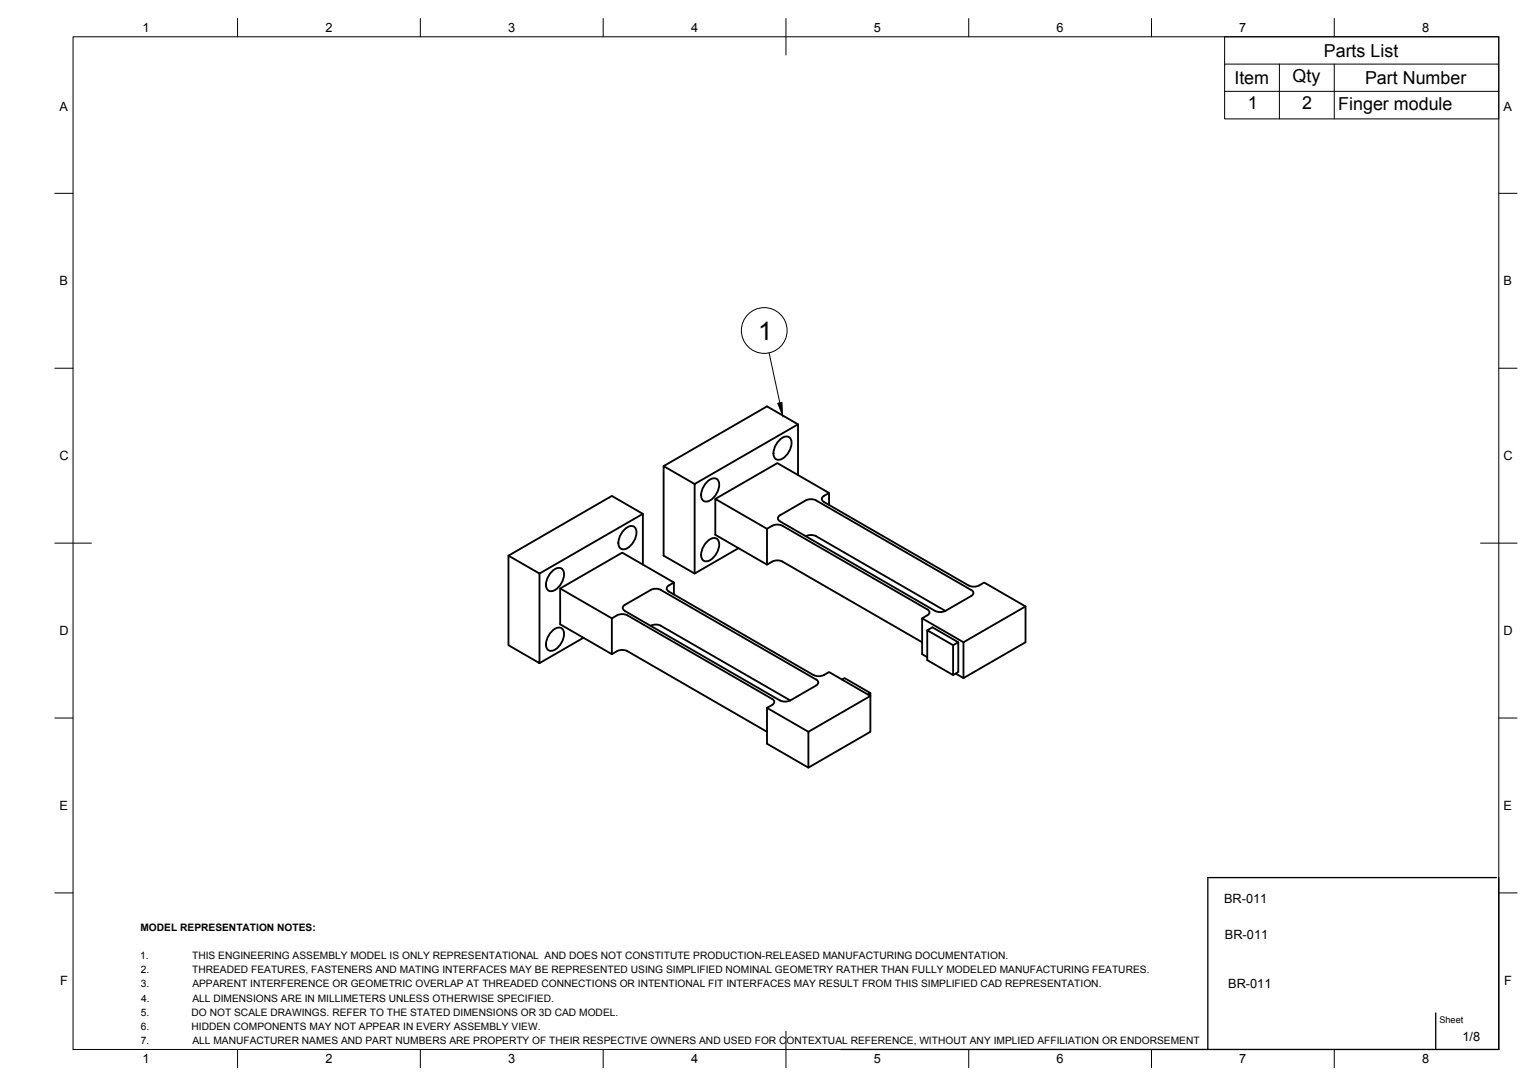
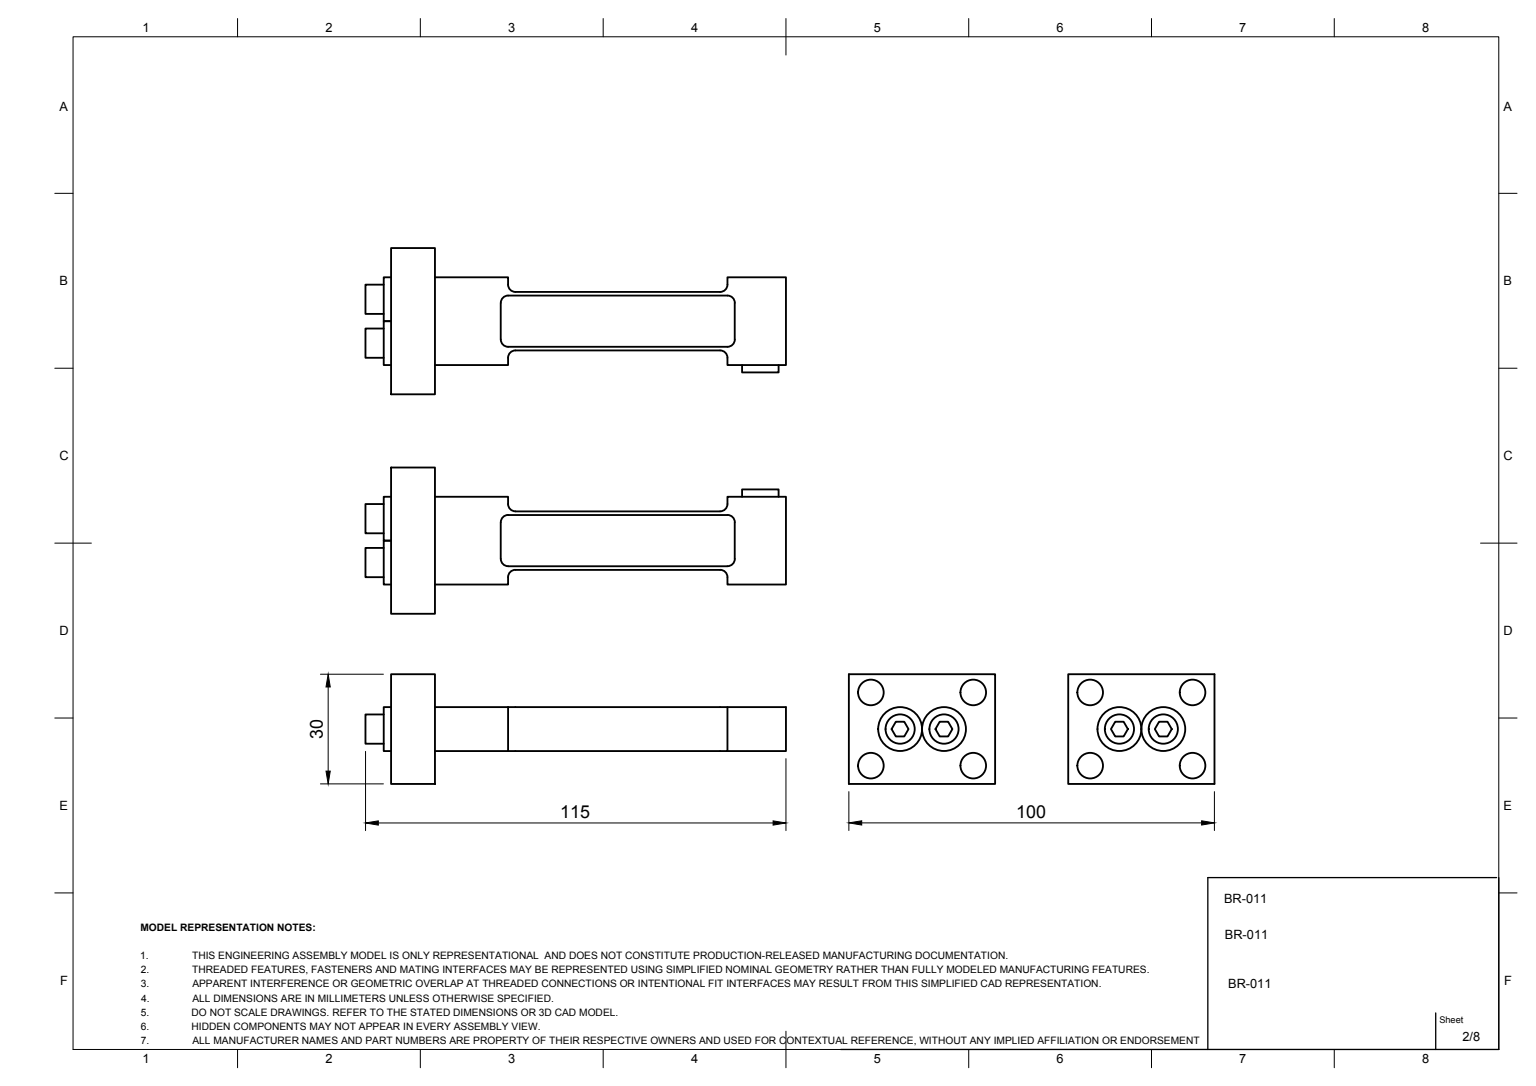
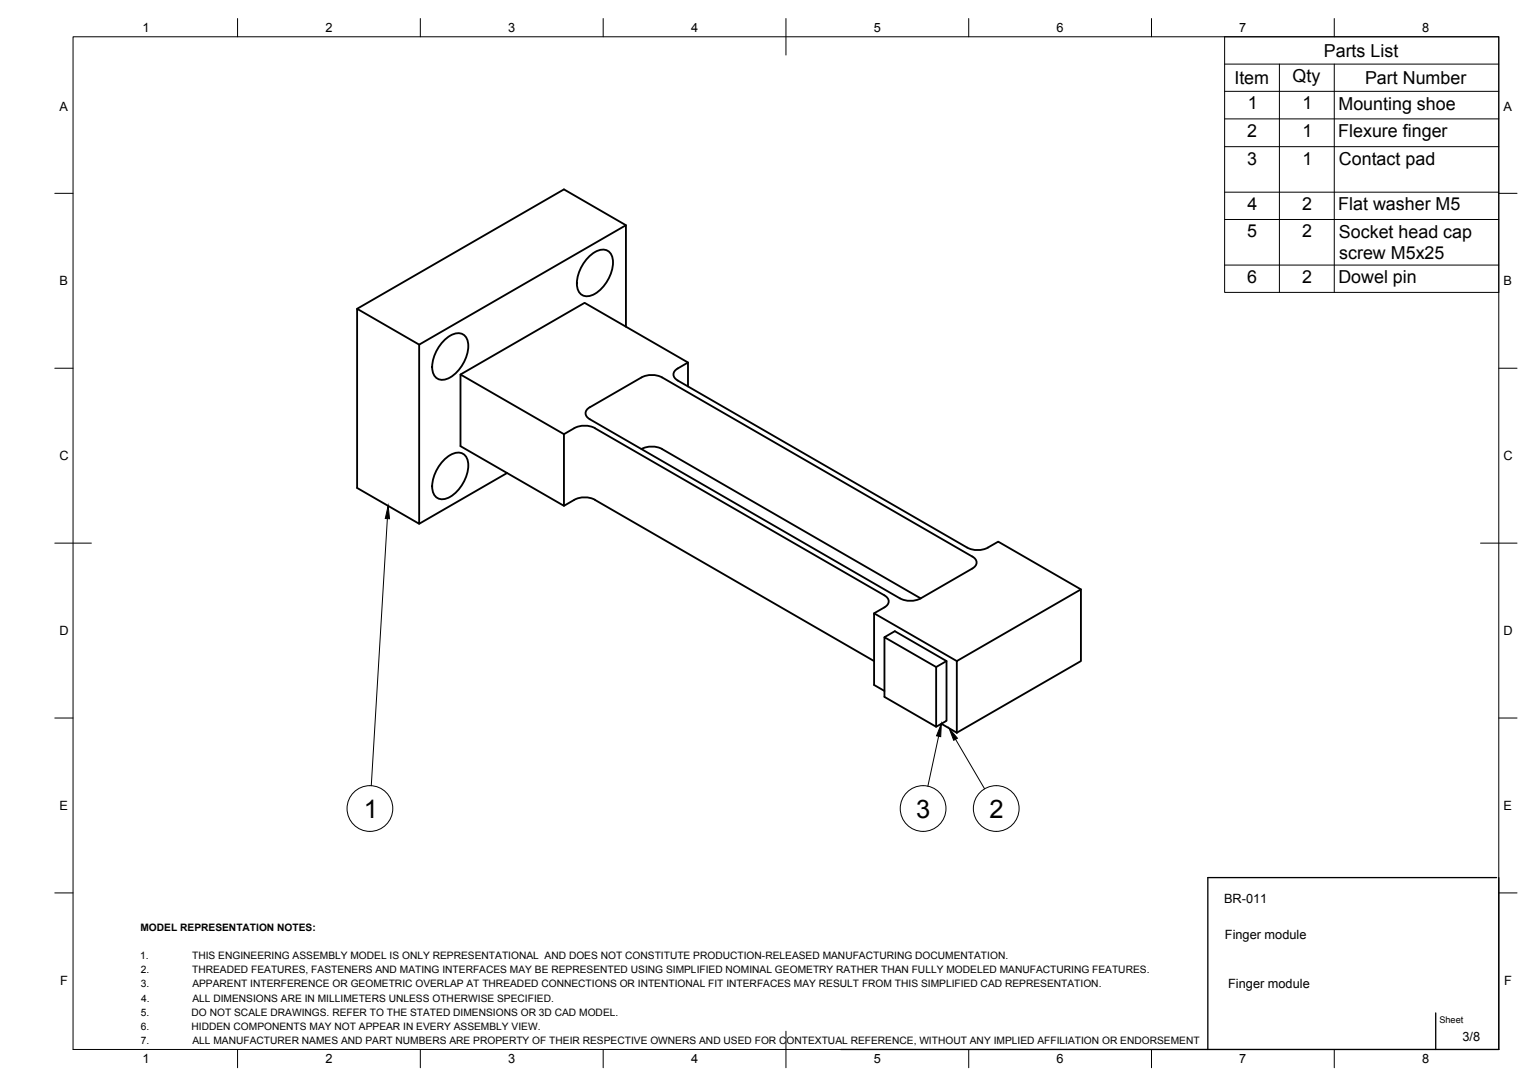
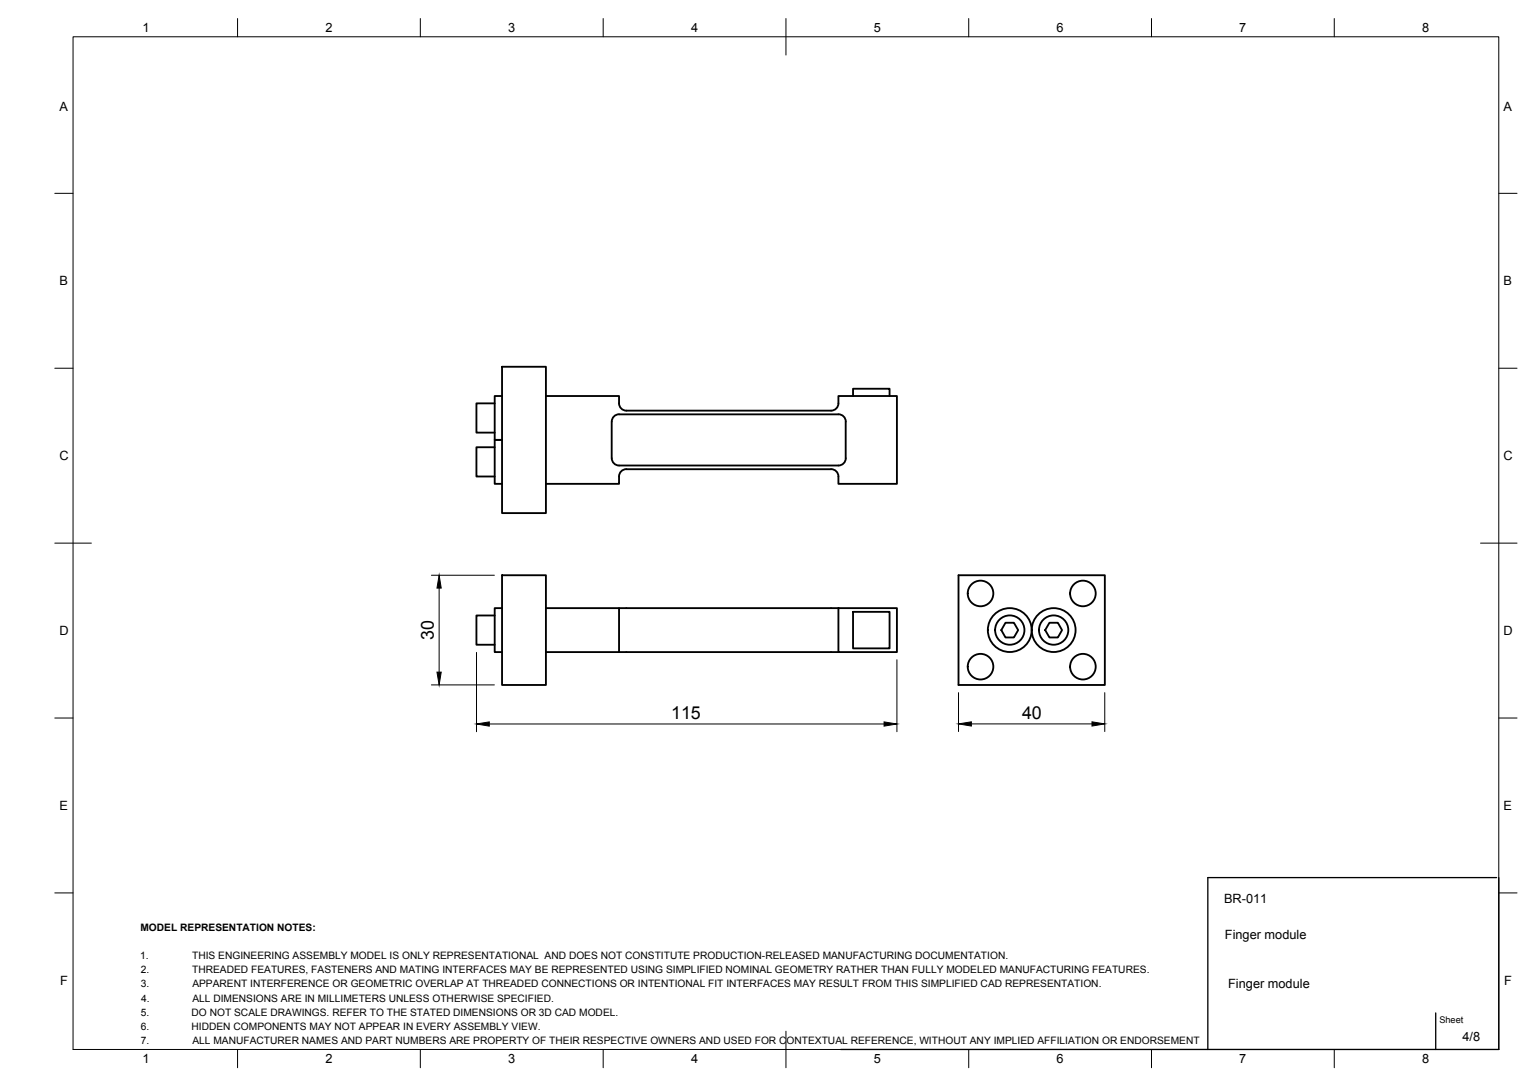
ISO-10303-21;
HEADER;
/* Generated by software containing ST-Developer
 * from STEP Tools, Inc. (www.steptools.com) 
 */

FILE_DESCRIPTION(
/* description */ ('Independent pair of monolithic parallel-leaf compliant finger modules.
 Shared native part/module instances; external gripper actuator outsid
e scope. Whole-mm geometry,1mm webs,56mm straight span,12mm depth,32mm
 nominal contact gap. Undeformed CAD reference; material condition, el
astic range, fatigue and gripping force unassigned.'),
/* implementation_level */ '2;1');

FILE_NAME(
/* name */ 'BR-011.step',
/* time_stamp */ '2026-11-07T22:36:16-08:00',
/* author */ (''),
/* organization */ (''),
/* preprocessor_version */ 'ST-DEVELOPER v20.2',
/* originating_system */ 'Autodesk Translation Framework v15.17.0.0',
/* authorisation */ '');

FILE_SCHEMA (('AUTOMOTIVE_DESIGN { 1 0 10303 214 3 1 1 }'));
ENDSEC;

DATA;
#10=MECHANICAL_DESIGN_GEOMETRIC_PRESENTATION_REPRESENTATION('',(#329,#330,
#331,#332,#333,#334),#13801);
#11=ITEM_DEFINED_TRANSFORMATION($,$,#3769,#4029);
#12=ITEM_DEFINED_TRANSFORMATION($,$,#3802,#4030);
#13=ITEM_DEFINED_TRANSFORMATION($,$,#3925,#4031);
#14=ITEM_DEFINED_TRANSFORMATION($,$,#3932,#4032);
#15=ITEM_DEFINED_TRANSFORMATION($,$,#3941,#4033);
#16=ITEM_DEFINED_TRANSFORMATION($,$,#4023,#4034);
#17=ITEM_DEFINED_TRANSFORMATION($,$,#3932,#4035);
#18=ITEM_DEFINED_TRANSFORMATION($,$,#3941,#4036);
#19=ITEM_DEFINED_TRANSFORMATION($,$,#4023,#4037);
#20=ITEM_DEFINED_TRANSFORMATION($,$,#3768,#4038);
#21=ITEM_DEFINED_TRANSFORMATION($,$,#3768,#4039);
#22=(
REPRESENTATION_RELATIONSHIP($,$,#13835,#13834)
REPRESENTATION_RELATIONSHIP_WITH_TRANSFORMATION(#11)
SHAPE_REPRESENTATION_RELATIONSHIP()
);
#23=(
REPRESENTATION_RELATIONSHIP($,$,#13836,#13834)
REPRESENTATION_RELATIONSHIP_WITH_TRANSFORMATION(#12)
SHAPE_REPRESENTATION_RELATIONSHIP()
);
#24=(
REPRESENTATION_RELATIONSHIP($,$,#13837,#13834)
REPRESENTATION_RELATIONSHIP_WITH_TRANSFORMATION(#13)
SHAPE_REPRESENTATION_RELATIONSHIP()
);
#25=(
REPRESENTATION_RELATIONSHIP($,$,#13838,#13834)
REPRESENTATION_RELATIONSHIP_WITH_TRANSFORMATION(#14)
SHAPE_REPRESENTATION_RELATIONSHIP()
);
#26=(
REPRESENTATION_RELATIONSHIP($,$,#13839,#13834)
REPRESENTATION_RELATIONSHIP_WITH_TRANSFORMATION(#15)
SHAPE_REPRESENTATION_RELATIONSHIP()
);
#27=(
REPRESENTATION_RELATIONSHIP($,$,#13840,#13834)
REPRESENTATION_RELATIONSHIP_WITH_TRANSFORMATION(#16)
SHAPE_REPRESENTATION_RELATIONSHIP()
);
#28=(
REPRESENTATION_RELATIONSHIP($,$,#13838,#13834)
REPRESENTATION_RELATIONSHIP_WITH_TRANSFORMATION(#17)
SHAPE_REPRESENTATION_RELATIONSHIP()
);
#29=(
REPRESENTATION_RELATIONSHIP($,$,#13839,#13834)
REPRESENTATION_RELATIONSHIP_WITH_TRANSFORMATION(#18)
SHAPE_REPRESENTATION_RELATIONSHIP()
);
#30=(
REPRESENTATION_RELATIONSHIP($,$,#13840,#13834)
REPRESENTATION_RELATIONSHIP_WITH_TRANSFORMATION(#19)
SHAPE_REPRESENTATION_RELATIONSHIP()
);
#31=(
REPRESENTATION_RELATIONSHIP($,$,#13834,#13833)
REPRESENTATION_RELATIONSHIP_WITH_TRANSFORMATION(#20)
SHAPE_REPRESENTATION_RELATIONSHIP()
);
#32=(
REPRESENTATION_RELATIONSHIP($,$,#13834,#13833)
REPRESENTATION_RELATIONSHIP_WITH_TRANSFORMATION(#21)
SHAPE_REPRESENTATION_RELATIONSHIP()
);
#33=CONTEXT_DEPENDENT_SHAPE_REPRESENTATION(#22,#13822);
#34=CONTEXT_DEPENDENT_SHAPE_REPRESENTATION(#23,#13823);
#35=CONTEXT_DEPENDENT_SHAPE_REPRESENTATION(#24,#13824);
#36=CONTEXT_DEPENDENT_SHAPE_REPRESENTATION(#25,#13825);
#37=CONTEXT_DEPENDENT_SHAPE_REPRESENTATION(#26,#13826);
#38=CONTEXT_DEPENDENT_SHAPE_REPRESENTATION(#27,#13827);
#39=CONTEXT_DEPENDENT_SHAPE_REPRESENTATION(#28,#13828);
#40=CONTEXT_DEPENDENT_SHAPE_REPRESENTATION(#29,#13829);
#41=CONTEXT_DEPENDENT_SHAPE_REPRESENTATION(#30,#13830);
#42=CONTEXT_DEPENDENT_SHAPE_REPRESENTATION(#31,#13831);
#43=CONTEXT_DEPENDENT_SHAPE_REPRESENTATION(#32,#13832);
#44=NEXT_ASSEMBLY_USAGE_OCCURRENCE('Mounting shoe:1','Mounting shoe:1',
'Mounting shoe:1',#13843,#13844,'Mounting shoe:1');
#45=NEXT_ASSEMBLY_USAGE_OCCURRENCE('Flexure finger:1',
'Flexure finger:1','Flexure finger:1',#13843,#13845,'Flexure finger:1');
#46=NEXT_ASSEMBLY_USAGE_OCCURRENCE('Contact pad:1','Contact pad:1',
'Contact pad:1',#13843,#13846,'Contact pad:1');
#47=NEXT_ASSEMBLY_USAGE_OCCURRENCE('Flat washer M5:1',
'Flat washer M5:1','Flat washer M5:1',#13843,#13847,'Flat washer M5:1');
#48=NEXT_ASSEMBLY_USAGE_OCCURRENCE('Socket head cap screw M5x25:1',
'Socket head cap screw M5x25:1','Socket head cap screw M5x25:1',#13843,
#13848,'Socket head cap screw M5x25:1');
#49=NEXT_ASSEMBLY_USAGE_OCCURRENCE('Dowel pin:1','Dowel pin:1',
'Dowel pin:1',#13843,#13849,'Dowel pin:1');
#50=NEXT_ASSEMBLY_USAGE_OCCURRENCE('Flat washer M5:2',
'Flat washer M5:2','Flat washer M5:2',#13843,#13847,'Flat washer M5:2');
#51=NEXT_ASSEMBLY_USAGE_OCCURRENCE('Socket head cap screw M5x25:2',
'Socket head cap screw M5x25:2','Socket head cap screw M5x25:2',#13843,
#13848,'Socket head cap screw M5x25:2');
#52=NEXT_ASSEMBLY_USAGE_OCCURRENCE('Dowel pin:2','Dowel pin:2',
'Dowel pin:2',#13843,#13849,'Dowel pin:2');
#53=NEXT_ASSEMBLY_USAGE_OCCURRENCE('Finger module:1','Finger module:1',
'Finger module:1',#13842,#13843,'Finger module:1');
#54=NEXT_ASSEMBLY_USAGE_OCCURRENCE('Finger module:2','Finger module:2',
'Finger module:2',#13842,#13843,'Finger module:2');
#55=CONICAL_SURFACE('',#4004,2.,0.785398163397448);
#56=B_SPLINE_SURFACE_WITH_KNOTS('',3,3,((#7071,#7072,#7073,#7074,#7075,
#7076,#7077,#7078,#7079,#7080,#7081,#7082,#7083,#7084,#7085,#7086,#7087,
#7088,#7089,#7090,#7091,#7092,#7093,#7094,#7095,#7096,#7097,#7098,#7099,
#7100,#7101,#7102,#7103,#7104,#7105,#7106,#7107,#7108,#7109,#7110,#7111,
#7112,#7113,#7114,#7115,#7116,#7117,#7118,#7119,#7120,#7121,#7122,#7123,
#7124,#7125,#7126,#7127,#7128,#7129,#7130,#7131,#7132,#7133,#7134,#7135,
#7136,#7137,#7138,#7139,#7140,#7141,#7142,#7143,#7144,#7145,#7146,#7147,
#7148,#7149,#7150,#7151,#7152,#7153,#7154,#7155,#7156,#7157,#7158,#7159,
#7160,#7161,#7162),(#7163,#7164,#7165,#7166,#7167,#7168,#7169,#7170,#7171,
#7172,#7173,#7174,#7175,#7176,#7177,#7178,#7179,#7180,#7181,#7182,#7183,
#7184,#7185,#7186,#7187,#7188,#7189,#7190,#7191,#7192,#7193,#7194,#7195,
#7196,#7197,#7198,#7199,#7200,#7201,#7202,#7203,#7204,#7205,#7206,#7207,
#7208,#7209,#7210,#7211,#7212,#7213,#7214,#7215,#7216,#7217,#7218,#7219,
#7220,#7221,#7222,#7223,#7224,#7225,#7226,#7227,#7228,#7229,#7230,#7231,
#7232,#7233,#7234,#7235,#7236,#7237,#7238,#7239,#7240,#7241,#7242,#7243,
#7244,#7245,#7246,#7247,#7248,#7249,#7250,#7251,#7252,#7253,#7254),(#7255,
#7256,#7257,#7258,#7259,#7260,#7261,#7262,#7263,#7264,#7265,#7266,#7267,
#7268,#7269,#7270,#7271,#7272,#7273,#7274,#7275,#7276,#7277,#7278,#7279,
#7280,#7281,#7282,#7283,#7284,#7285,#7286,#7287,#7288,#7289,#7290,#7291,
#7292,#7293,#7294,#7295,#7296,#7297,#7298,#7299,#7300,#7301,#7302,#7303,
#7304,#7305,#7306,#7307,#7308,#7309,#7310,#7311,#7312,#7313,#7314,#7315,
#7316,#7317,#7318,#7319,#7320,#7321,#7322,#7323,#7324,#7325,#7326,#7327,
#7328,#7329,#7330,#7331,#7332,#7333,#7334,#7335,#7336,#7337,#7338,#7339,
#7340,#7341,#7342,#7343,#7344,#7345,#7346),(#7347,#7348,#7349,#7350,#7351,
#7352,#7353,#7354,#7355,#7356,#7357,#7358,#7359,#7360,#7361,#7362,#7363,
#7364,#7365,#7366,#7367,#7368,#7369,#7370,#7371,#7372,#7373,#7374,#7375,
#7376,#7377,#7378,#7379,#7380,#7381,#7382,#7383,#7384,#7385,#7386,#7387,
#7388,#7389,#7390,#7391,#7392,#7393,#7394,#7395,#7396,#7397,#7398,#7399,
#7400,#7401,#7402,#7403,#7404,#7405,#7406,#7407,#7408,#7409,#7410,#7411,
#7412,#7413,#7414,#7415,#7416,#7417,#7418,#7419,#7420,#7421,#7422,#7423,
#7424,#7425,#7426,#7427,#7428,#7429,#7430,#7431,#7432,#7433,#7434,#7435,
#7436,#7437,#7438)),.UNSPECIFIED.,.F.,.F.,.F.,(4,4),(4,1,1,1,1,1,1,1,1,
1,1,1,1,1,1,1,1,1,1,1,1,1,1,1,1,1,1,1,1,1,1,1,1,1,1,1,1,1,1,1,1,1,1,1,1,
1,1,1,1,1,1,1,1,1,1,1,1,1,1,1,1,1,1,1,1,1,1,1,1,1,1,1,1,1,1,1,1,1,1,1,1,
1,1,1,1,1,1,1,1,4),(0.,0.0511532338502008),(11.8669242345263,12.8602116589039,
13.8534990832815,14.8467865076592,15.8400739320368,16.8333613564144,17.826648780792,
18.8199362051697,19.8132236295473,20.8065110539249,21.7997984783025,22.7930859026802,
23.7863733270578,24.7796607514354,25.772948175813,26.7662356001907,27.7595230245683,
28.7528104489459,29.7460978733235,30.7393852977012,31.7326727220788,32.7259601464564,
33.719247570834,34.7125349952117,35.7058224195893,36.6991098439669,37.6923972683445,
38.6856846927222,39.6789721170998,40.6722595414774,41.6655469658551,42.6588343902327,
43.6521218146103,44.6454092389879,45.6386966633656,46.6319840877432,47.6252715121208,
48.6185589364984,49.6118463608761,50.6051337852537,51.5984212096313,52.5917086340089,
53.5849960583866,54.5782834827642,55.5715709071418,56.5648583315194,57.5581457558971,
58.5514331802747,59.5447206046523,60.5380080290299,61.5312954534076,62.5245828777852,
63.5178703021628,64.5111577265404,65.5044451509181,66.4977325752957,67.4910199996733,
68.4843074240509,69.4775948484286,70.4708822728062,71.4641696971838,72.4574571215614,
73.4507445459391,74.4440319703167,75.4373193946943,76.430606819072,77.4238942434496,
78.4171816678272,79.4104690922048,80.4037565165825,81.3970439409601,82.3903313653377,
83.3836187897153,84.376906214093,85.3701936384706,86.3634810628482,87.3567684872258,
88.3500559116035,89.3433433359811,90.3366307603587,91.3299181847363,92.323205609114,
93.3164930334916,94.3097804578692,95.3030678822468,96.2963553066245,97.2896427310021,
98.2829301553797,99.2762175797573,100.269505004135),.UNSPECIFIED.);
#57=B_SPLINE_SURFACE_WITH_KNOTS('',3,3,((#7555,#7556,#7557,#7558,#7559,
#7560,#7561,#7562,#7563,#7564,#7565,#7566,#7567,#7568,#7569,#7570,#7571,
#7572,#7573,#7574,#7575,#7576,#7577,#7578,#7579,#7580,#7581,#7582,#7583,
#7584,#7585,#7586,#7587,#7588,#7589,#7590,#7591,#7592,#7593,#7594,#7595,
#7596,#7597,#7598,#7599,#7600,#7601,#7602,#7603,#7604,#7605,#7606,#7607,
#7608,#7609,#7610,#7611,#7612,#7613,#7614,#7615,#7616,#7617,#7618,#7619,
#7620,#7621,#7622,#7623,#7624,#7625,#7626,#7627,#7628,#7629,#7630,#7631,
#7632,#7633,#7634,#7635,#7636,#7637,#7638,#7639,#7640,#7641,#7642,#7643,
#7644,#7645,#7646),(#7647,#7648,#7649,#7650,#7651,#7652,#7653,#7654,#7655,
#7656,#7657,#7658,#7659,#7660,#7661,#7662,#7663,#7664,#7665,#7666,#7667,
#7668,#7669,#7670,#7671,#7672,#7673,#7674,#7675,#7676,#7677,#7678,#7679,
#7680,#7681,#7682,#7683,#7684,#7685,#7686,#7687,#7688,#7689,#7690,#7691,
#7692,#7693,#7694,#7695,#7696,#7697,#7698,#7699,#7700,#7701,#7702,#7703,
#7704,#7705,#7706,#7707,#7708,#7709,#7710,#7711,#7712,#7713,#7714,#7715,
#7716,#7717,#7718,#7719,#7720,#7721,#7722,#7723,#7724,#7725,#7726,#7727,
#7728,#7729,#7730,#7731,#7732,#7733,#7734,#7735,#7736,#7737,#7738),(#7739,
#7740,#7741,#7742,#7743,#7744,#7745,#7746,#7747,#7748,#7749,#7750,#7751,
#7752,#7753,#7754,#7755,#7756,#7757,#7758,#7759,#7760,#7761,#7762,#7763,
#7764,#7765,#7766,#7767,#7768,#7769,#7770,#7771,#7772,#7773,#7774,#7775,
#7776,#7777,#7778,#7779,#7780,#7781,#7782,#7783,#7784,#7785,#7786,#7787,
#7788,#7789,#7790,#7791,#7792,#7793,#7794,#7795,#7796,#7797,#7798,#7799,
#7800,#7801,#7802,#7803,#7804,#7805,#7806,#7807,#7808,#7809,#7810,#7811,
#7812,#7813,#7814,#7815,#7816,#7817,#7818,#7819,#7820,#7821,#7822,#7823,
#7824,#7825,#7826,#7827,#7828,#7829,#7830),(#7831,#7832,#7833,#7834,#7835,
#7836,#7837,#7838,#7839,#7840,#7841,#7842,#7843,#7844,#7845,#7846,#7847,
#7848,#7849,#7850,#7851,#7852,#7853,#7854,#7855,#7856,#7857,#7858,#7859,
#7860,#7861,#7862,#7863,#7864,#7865,#7866,#7867,#7868,#7869,#7870,#7871,
#7872,#7873,#7874,#7875,#7876,#7877,#7878,#7879,#7880,#7881,#7882,#7883,
#7884,#7885,#7886,#7887,#7888,#7889,#7890,#7891,#7892,#7893,#7894,#7895,
#7896,#7897,#7898,#7899,#7900,#7901,#7902,#7903,#7904,#7905,#7906,#7907,
#7908,#7909,#7910,#7911,#7912,#7913,#7914,#7915,#7916,#7917,#7918,#7919,
#7920,#7921,#7922)),.UNSPECIFIED.,.F.,.F.,.F.,(4,4),(4,1,1,1,1,1,1,1,1,
1,1,1,1,1,1,1,1,1,1,1,1,1,1,1,1,1,1,1,1,1,1,1,1,1,1,1,1,1,1,1,1,1,1,1,1,
1,1,1,1,1,1,1,1,1,1,1,1,1,1,1,1,1,1,1,1,1,1,1,1,1,1,1,1,1,1,1,1,1,1,1,1,
1,1,1,1,1,1,1,1,4),(0.,0.0511532338502008),(14.3986268518923,15.3919142762699,
16.3852017006476,17.3784891250252,18.3717765494028,19.3650639737804,20.3583513981581,
21.3516388225357,22.3449262469133,23.3382136712909,24.3315010956686,25.3247885200462,
26.3180759444238,27.3113633688014,28.3046507931791,29.2979382175567,30.2912256419343,
31.284513066312,32.2778004906896,33.2710879150672,34.2643753394448,35.2576627638225,
36.2509501882001,37.2442376125777,38.2375250369553,39.230812461333,40.2240998857106,
41.2173873100882,42.2106747344658,43.2039621588435,44.1972495832211,45.1905370075987,
46.1838244319763,47.177111856354,48.1703992807316,49.1636867051092,50.1569741294868,
51.1502615538645,52.1435489782421,53.1368364026197,54.1301238269973,55.123411251375,
56.1166986757526,57.1099861001302,58.1032735245078,59.0965609488855,60.0898483732631,
61.0831357976407,62.0764232220183,63.069710646396,64.0629980707736,65.0562854951512,
66.0495729195289,67.0428603439065,68.0361477682841,69.0294351926617,70.0227226170393,
71.016010041417,72.0092974657946,73.0025848901722,73.9958723145499,74.9891597389275,
75.9824471633051,76.9757345876827,77.9690220120604,78.962309436438,79.9555968608156,
80.9488842851932,81.9421717095709,82.9354591339485,83.9287465583261,84.9220339827037,
85.9153214070814,86.908608831459,87.9018962558366,88.8951836802142,89.8884711045919,
90.8817585289695,91.8750459533471,92.8683333777248,93.8616208021024,94.85490822648,
95.8481956508576,96.8414830752353,97.8347704996129,98.8280579239905,99.8213453483681,
100.814632772746,101.807920197123,102.801207621501),.UNSPECIFIED.);
#58=B_SPLINE_SURFACE_WITH_KNOTS('',3,3,((#8239,#8240,#8241,#8242,#8243,
#8244,#8245,#8246,#8247,#8248,#8249,#8250,#8251,#8252,#8253,#8254,#8255,
#8256,#8257,#8258,#8259,#8260,#8261,#8262,#8263,#8264,#8265,#8266,#8267,
#8268,#8269,#8270,#8271,#8272,#8273,#8274,#8275,#8276,#8277,#8278,#8279,
#8280,#8281,#8282,#8283,#8284,#8285,#8286,#8287,#8288,#8289,#8290,#8291,
#8292,#8293,#8294,#8295,#8296,#8297,#8298,#8299,#8300,#8301,#8302,#8303,
#8304,#8305,#8306,#8307,#8308,#8309,#8310,#8311,#8312,#8313,#8314,#8315,
#8316,#8317,#8318,#8319,#8320,#8321,#8322,#8323,#8324,#8325,#8326,#8327,
#8328,#8329,#8330),(#8331,#8332,#8333,#8334,#8335,#8336,#8337,#8338,#8339,
#8340,#8341,#8342,#8343,#8344,#8345,#8346,#8347,#8348,#8349,#8350,#8351,
#8352,#8353,#8354,#8355,#8356,#8357,#8358,#8359,#8360,#8361,#8362,#8363,
#8364,#8365,#8366,#8367,#8368,#8369,#8370,#8371,#8372,#8373,#8374,#8375,
#8376,#8377,#8378,#8379,#8380,#8381,#8382,#8383,#8384,#8385,#8386,#8387,
#8388,#8389,#8390,#8391,#8392,#8393,#8394,#8395,#8396,#8397,#8398,#8399,
#8400,#8401,#8402,#8403,#8404,#8405,#8406,#8407,#8408,#8409,#8410,#8411,
#8412,#8413,#8414,#8415,#8416,#8417,#8418,#8419,#8420,#8421,#8422),(#8423,
#8424,#8425,#8426,#8427,#8428,#8429,#8430,#8431,#8432,#8433,#8434,#8435,
#8436,#8437,#8438,#8439,#8440,#8441,#8442,#8443,#8444,#8445,#8446,#8447,
#8448,#8449,#8450,#8451,#8452,#8453,#8454,#8455,#8456,#8457,#8458,#8459,
#8460,#8461,#8462,#8463,#8464,#8465,#8466,#8467,#8468,#8469,#8470,#8471,
#8472,#8473,#8474,#8475,#8476,#8477,#8478,#8479,#8480,#8481,#8482,#8483,
#8484,#8485,#8486,#8487,#8488,#8489,#8490,#8491,#8492,#8493,#8494,#8495,
#8496,#8497,#8498,#8499,#8500,#8501,#8502,#8503,#8504,#8505,#8506,#8507,
#8508,#8509,#8510,#8511,#8512,#8513,#8514),(#8515,#8516,#8517,#8518,#8519,
#8520,#8521,#8522,#8523,#8524,#8525,#8526,#8527,#8528,#8529,#8530,#8531,
#8532,#8533,#8534,#8535,#8536,#8537,#8538,#8539,#8540,#8541,#8542,#8543,
#8544,#8545,#8546,#8547,#8548,#8549,#8550,#8551,#8552,#8553,#8554,#8555,
#8556,#8557,#8558,#8559,#8560,#8561,#8562,#8563,#8564,#8565,#8566,#8567,
#8568,#8569,#8570,#8571,#8572,#8573,#8574,#8575,#8576,#8577,#8578,#8579,
#8580,#8581,#8582,#8583,#8584,#8585,#8586,#8587,#8588,#8589,#8590,#8591,
#8592,#8593,#8594,#8595,#8596,#8597,#8598,#8599,#8600,#8601,#8602,#8603,
#8604,#8605,#8606)),.UNSPECIFIED.,.F.,.F.,.F.,(4,4),(4,1,1,1,1,1,1,1,1,
1,1,1,1,1,1,1,1,1,1,1,1,1,1,1,1,1,1,1,1,1,1,1,1,1,1,1,1,1,1,1,1,1,1,1,1,
1,1,1,1,1,1,1,1,1,1,1,1,1,1,1,1,1,1,1,1,1,1,1,1,1,1,1,1,1,1,1,1,1,1,1,1,
1,1,1,1,1,1,1,1,4),(0.,0.0511532338502008),(11.8669242345263,12.8602116589039,
13.8534990832815,14.8467865076592,15.8400739320368,16.8333613564144,17.826648780792,
18.8199362051697,19.8132236295473,20.8065110539249,21.7997984783025,22.7930859026802,
23.7863733270578,24.7796607514354,25.772948175813,26.7662356001907,27.7595230245683,
28.7528104489459,29.7460978733235,30.7393852977012,31.7326727220788,32.7259601464564,
33.719247570834,34.7125349952117,35.7058224195893,36.6991098439669,37.6923972683445,
38.6856846927222,39.6789721170998,40.6722595414774,41.6655469658551,42.6588343902327,
43.6521218146103,44.6454092389879,45.6386966633656,46.6319840877432,47.6252715121208,
48.6185589364984,49.6118463608761,50.6051337852537,51.5984212096313,52.5917086340089,
53.5849960583866,54.5782834827642,55.5715709071418,56.5648583315194,57.5581457558971,
58.5514331802747,59.5447206046523,60.5380080290299,61.5312954534076,62.5245828777852,
63.5178703021628,64.5111577265404,65.5044451509181,66.4977325752957,67.4910199996733,
68.4843074240509,69.4775948484286,70.4708822728062,71.4641696971838,72.4574571215614,
73.4507445459391,74.4440319703167,75.4373193946943,76.430606819072,77.4238942434496,
78.4171816678272,79.4104690922048,80.4037565165825,81.3970439409601,82.3903313653377,
83.3836187897153,84.376906214093,85.3701936384706,86.3634810628482,87.3567684872258,
88.3500559116035,89.3433433359811,90.3366307603587,91.3299181847363,92.323205609114,
93.3164930334916,94.3097804578692,95.3030678822468,96.2963553066245,97.2896427310021,
98.2829301553797,99.2762175797573,100.269505004135),.UNSPECIFIED.);
#59=B_SPLINE_SURFACE_WITH_KNOTS('',3,3,((#8723,#8724,#8725,#8726,#8727,
#8728,#8729,#8730,#8731,#8732,#8733,#8734,#8735,#8736,#8737,#8738,#8739,
#8740,#8741,#8742,#8743,#8744,#8745,#8746,#8747,#8748,#8749,#8750,#8751,
#8752,#8753,#8754,#8755,#8756,#8757,#8758,#8759,#8760,#8761,#8762,#8763,
#8764,#8765,#8766,#8767,#8768,#8769,#8770,#8771,#8772,#8773,#8774,#8775,
#8776,#8777,#8778,#8779,#8780,#8781,#8782,#8783,#8784,#8785,#8786,#8787,
#8788,#8789,#8790,#8791,#8792,#8793,#8794,#8795,#8796,#8797,#8798,#8799,
#8800,#8801,#8802,#8803,#8804,#8805,#8806,#8807,#8808,#8809,#8810,#8811,
#8812,#8813,#8814),(#8815,#8816,#8817,#8818,#8819,#8820,#8821,#8822,#8823,
#8824,#8825,#8826,#8827,#8828,#8829,#8830,#8831,#8832,#8833,#8834,#8835,
#8836,#8837,#8838,#8839,#8840,#8841,#8842,#8843,#8844,#8845,#8846,#8847,
#8848,#8849,#8850,#8851,#8852,#8853,#8854,#8855,#8856,#8857,#8858,#8859,
#8860,#8861,#8862,#8863,#8864,#8865,#8866,#8867,#8868,#8869,#8870,#8871,
#8872,#8873,#8874,#8875,#8876,#8877,#8878,#8879,#8880,#8881,#8882,#8883,
#8884,#8885,#8886,#8887,#8888,#8889,#8890,#8891,#8892,#8893,#8894,#8895,
#8896,#8897,#8898,#8899,#8900,#8901,#8902,#8903,#8904,#8905,#8906),(#8907,
#8908,#8909,#8910,#8911,#8912,#8913,#8914,#8915,#8916,#8917,#8918,#8919,
#8920,#8921,#8922,#8923,#8924,#8925,#8926,#8927,#8928,#8929,#8930,#8931,
#8932,#8933,#8934,#8935,#8936,#8937,#8938,#8939,#8940,#8941,#8942,#8943,
#8944,#8945,#8946,#8947,#8948,#8949,#8950,#8951,#8952,#8953,#8954,#8955,
#8956,#8957,#8958,#8959,#8960,#8961,#8962,#8963,#8964,#8965,#8966,#8967,
#8968,#8969,#8970,#8971,#8972,#8973,#8974,#8975,#8976,#8977,#8978,#8979,
#8980,#8981,#8982,#8983,#8984,#8985,#8986,#8987,#8988,#8989,#8990,#8991,
#8992,#8993,#8994,#8995,#8996,#8997,#8998),(#8999,#9000,#9001,#9002,#9003,
#9004,#9005,#9006,#9007,#9008,#9009,#9010,#9011,#9012,#9013,#9014,#9015,
#9016,#9017,#9018,#9019,#9020,#9021,#9022,#9023,#9024,#9025,#9026,#9027,
#9028,#9029,#9030,#9031,#9032,#9033,#9034,#9035,#9036,#9037,#9038,#9039,
#9040,#9041,#9042,#9043,#9044,#9045,#9046,#9047,#9048,#9049,#9050,#9051,
#9052,#9053,#9054,#9055,#9056,#9057,#9058,#9059,#9060,#9061,#9062,#9063,
#9064,#9065,#9066,#9067,#9068,#9069,#9070,#9071,#9072,#9073,#9074,#9075,
#9076,#9077,#9078,#9079,#9080,#9081,#9082,#9083,#9084,#9085,#9086,#9087,
#9088,#9089,#9090)),.UNSPECIFIED.,.F.,.F.,.F.,(4,4),(4,1,1,1,1,1,1,1,1,
1,1,1,1,1,1,1,1,1,1,1,1,1,1,1,1,1,1,1,1,1,1,1,1,1,1,1,1,1,1,1,1,1,1,1,1,
1,1,1,1,1,1,1,1,1,1,1,1,1,1,1,1,1,1,1,1,1,1,1,1,1,1,1,1,1,1,1,1,1,1,1,1,
1,1,1,1,1,1,1,1,4),(0.,0.0511532338502008),(14.3986268518923,15.3919142762699,
16.3852017006476,17.3784891250252,18.3717765494028,19.3650639737804,20.3583513981581,
21.3516388225357,22.3449262469133,23.3382136712909,24.3315010956686,25.3247885200462,
26.3180759444238,27.3113633688014,28.3046507931791,29.2979382175567,30.2912256419343,
31.284513066312,32.2778004906896,33.2710879150672,34.2643753394448,35.2576627638225,
36.2509501882001,37.2442376125777,38.2375250369553,39.230812461333,40.2240998857106,
41.2173873100882,42.2106747344658,43.2039621588435,44.1972495832211,45.1905370075987,
46.1838244319763,47.177111856354,48.1703992807316,49.1636867051092,50.1569741294868,
51.1502615538645,52.1435489782421,53.1368364026197,54.1301238269973,55.123411251375,
56.1166986757526,57.1099861001302,58.1032735245078,59.0965609488855,60.0898483732631,
61.0831357976407,62.0764232220183,63.069710646396,64.0629980707736,65.0562854951512,
66.0495729195289,67.0428603439065,68.0361477682841,69.0294351926617,70.0227226170393,
71.016010041417,72.0092974657946,73.0025848901722,73.9958723145499,74.9891597389275,
75.9824471633051,76.9757345876827,77.9690220120604,78.962309436438,79.9555968608156,
80.9488842851932,81.9421717095709,82.9354591339485,83.9287465583261,84.9220339827037,
85.9153214070814,86.908608831459,87.9018962558366,88.8951836802142,89.8884711045919,
90.8817585289695,91.8750459533471,92.8683333777248,93.8616208021024,94.85490822648,
95.8481956508576,96.8414830752353,97.8347704996129,98.8280579239905,99.8213453483681,
100.814632772746,101.807920197123,102.801207621501),.UNSPECIFIED.);
#60=B_SPLINE_SURFACE_WITH_KNOTS('',3,3,((#11906,#11907,#11908,#11909,#11910,
#11911,#11912,#11913,#11914,#11915,#11916,#11917,#11918,#11919,#11920,#11921,
#11922,#11923,#11924,#11925,#11926,#11927,#11928,#11929,#11930,#11931,#11932,
#11933,#11934,#11935,#11936,#11937,#11938,#11939,#11940,#11941,#11942,#11943,
#11944,#11945,#11946,#11947,#11948,#11949,#11950,#11951,#11952,#11953,#11954,
#11955,#11956,#11957,#11958,#11959,#11960,#11961,#11962,#11963,#11964,#11965,
#11966,#11967,#11968,#11969,#11970,#11971,#11972,#11973,#11974,#11975,#11976,
#11977,#11978,#11979,#11980,#11981,#11982,#11983,#11984,#11985,#11986,#11987,
#11988,#11989,#11990,#11991,#11992,#11993,#11994,#11995,#11996,#11997,#11998,
#11999,#12000,#12001,#12002,#12003,#12004,#12005,#12006,#12007,#12008,#12009,
#12010,#12011,#12012,#12013,#12014,#12015,#12016,#12017,#12018,#12019,#12020,
#12021,#12022,#12023,#12024,#12025,#12026,#12027,#12028,#12029,#12030,#12031,
#12032,#12033,#12034,#12035,#12036,#12037,#12038,#12039,#12040,#12041,#12042,
#12043,#12044,#12045,#12046,#12047,#12048,#12049,#12050,#12051,#12052,#12053,
#12054,#12055,#12056,#12057,#12058,#12059,#12060,#12061,#12062,#12063,#12064,
#12065,#12066,#12067,#12068,#12069,#12070,#12071,#12072,#12073,#12074,#12075,
#12076,#12077,#12078,#12079,#12080,#12081,#12082,#12083,#12084,#12085,#12086,
#12087,#12088,#12089,#12090,#12091,#12092,#12093,#12094,#12095,#12096,#12097,
#12098,#12099,#12100,#12101),(#12102,#12103,#12104,#12105,#12106,#12107,
#12108,#12109,#12110,#12111,#12112,#12113,#12114,#12115,#12116,#12117,#12118,
#12119,#12120,#12121,#12122,#12123,#12124,#12125,#12126,#12127,#12128,#12129,
#12130,#12131,#12132,#12133,#12134,#12135,#12136,#12137,#12138,#12139,#12140,
#12141,#12142,#12143,#12144,#12145,#12146,#12147,#12148,#12149,#12150,#12151,
#12152,#12153,#12154,#12155,#12156,#12157,#12158,#12159,#12160,#12161,#12162,
#12163,#12164,#12165,#12166,#12167,#12168,#12169,#12170,#12171,#12172,#12173,
#12174,#12175,#12176,#12177,#12178,#12179,#12180,#12181,#12182,#12183,#12184,
#12185,#12186,#12187,#12188,#12189,#12190,#12191,#12192,#12193,#12194,#12195,
#12196,#12197,#12198,#12199,#12200,#12201,#12202,#12203,#12204,#12205,#12206,
#12207,#12208,#12209,#12210,#12211,#12212,#12213,#12214,#12215,#12216,#12217,
#12218,#12219,#12220,#12221,#12222,#12223,#12224,#12225,#12226,#12227,#12228,
#12229,#12230,#12231,#12232,#12233,#12234,#12235,#12236,#12237,#12238,#12239,
#12240,#12241,#12242,#12243,#12244,#12245,#12246,#12247,#12248,#12249,#12250,
#12251,#12252,#12253,#12254,#12255,#12256,#12257,#12258,#12259,#12260,#12261,
#12262,#12263,#12264,#12265,#12266,#12267,#12268,#12269,#12270,#12271,#12272,
#12273,#12274,#12275,#12276,#12277,#12278,#12279,#12280,#12281,#12282,#12283,
#12284,#12285,#12286,#12287,#12288,#12289,#12290,#12291,#12292,#12293,#12294,
#12295,#12296,#12297),(#12298,#12299,#12300,#12301,#12302,#12303,#12304,
#12305,#12306,#12307,#12308,#12309,#12310,#12311,#12312,#12313,#12314,#12315,
#12316,#12317,#12318,#12319,#12320,#12321,#12322,#12323,#12324,#12325,#12326,
#12327,#12328,#12329,#12330,#12331,#12332,#12333,#12334,#12335,#12336,#12337,
#12338,#12339,#12340,#12341,#12342,#12343,#12344,#12345,#12346,#12347,#12348,
#12349,#12350,#12351,#12352,#12353,#12354,#12355,#12356,#12357,#12358,#12359,
#12360,#12361,#12362,#12363,#12364,#12365,#12366,#12367,#12368,#12369,#12370,
#12371,#12372,#12373,#12374,#12375,#12376,#12377,#12378,#12379,#12380,#12381,
#12382,#12383,#12384,#12385,#12386,#12387,#12388,#12389,#12390,#12391,#12392,
#12393,#12394,#12395,#12396,#12397,#12398,#12399,#12400,#12401,#12402,#12403,
#12404,#12405,#12406,#12407,#12408,#12409,#12410,#12411,#12412,#12413,#12414,
#12415,#12416,#12417,#12418,#12419,#12420,#12421,#12422,#12423,#12424,#12425,
#12426,#12427,#12428,#12429,#12430,#12431,#12432,#12433,#12434,#12435,#12436,
#12437,#12438,#12439,#12440,#12441,#12442,#12443,#12444,#12445,#12446,#12447,
#12448,#12449,#12450,#12451,#12452,#12453,#12454,#12455,#12456,#12457,#12458,
#12459,#12460,#12461,#12462,#12463,#12464,#12465,#12466,#12467,#12468,#12469,
#12470,#12471,#12472,#12473,#12474,#12475,#12476,#12477,#12478,#12479,#12480,
#12481,#12482,#12483,#12484,#12485,#12486,#12487,#12488,#12489,#12490,#12491,
#12492,#12493),(#12494,#12495,#12496,#12497,#12498,#12499,#12500,#12501,
#12502,#12503,#12504,#12505,#12506,#12507,#12508,#12509,#12510,#12511,#12512,
#12513,#12514,#12515,#12516,#12517,#12518,#12519,#12520,#12521,#12522,#12523,
#12524,#12525,#12526,#12527,#12528,#12529,#12530,#12531,#12532,#12533,#12534,
#12535,#12536,#12537,#12538,#12539,#12540,#12541,#12542,#12543,#12544,#12545,
#12546,#12547,#12548,#12549,#12550,#12551,#12552,#12553,#12554,#12555,#12556,
#12557,#12558,#12559,#12560,#12561,#12562,#12563,#12564,#12565,#12566,#12567,
#12568,#12569,#12570,#12571,#12572,#12573,#12574,#12575,#12576,#12577,#12578,
#12579,#12580,#12581,#12582,#12583,#12584,#12585,#12586,#12587,#12588,#12589,
#12590,#12591,#12592,#12593,#12594,#12595,#12596,#12597,#12598,#12599,#12600,
#12601,#12602,#12603,#12604,#12605,#12606,#12607,#12608,#12609,#12610,#12611,
#12612,#12613,#12614,#12615,#12616,#12617,#12618,#12619,#12620,#12621,#12622,
#12623,#12624,#12625,#12626,#12627,#12628,#12629,#12630,#12631,#12632,#12633,
#12634,#12635,#12636,#12637,#12638,#12639,#12640,#12641,#12642,#12643,#12644,
#12645,#12646,#12647,#12648,#12649,#12650,#12651,#12652,#12653,#12654,#12655,
#12656,#12657,#12658,#12659,#12660,#12661,#12662,#12663,#12664,#12665,#12666,
#12667,#12668,#12669,#12670,#12671,#12672,#12673,#12674,#12675,#12676,#12677,
#12678,#12679,#12680,#12681,#12682,#12683,#12684,#12685,#12686,#12687,#12688,
#12689)),.UNSPECIFIED.,.F.,.F.,.F.,(4,4),(4,1,1,1,1,1,1,1,1,1,1,1,1,1,1,
1,1,1,1,1,1,1,1,1,1,1,1,1,1,1,1,1,1,1,1,1,1,1,1,1,1,1,1,1,1,1,1,1,1,1,1,
1,1,1,1,1,1,1,1,1,1,1,1,1,1,1,1,1,1,1,1,1,1,1,1,1,1,1,1,1,1,1,1,1,1,1,1,
1,1,1,1,1,1,1,1,1,1,1,1,1,1,1,1,1,1,1,1,1,1,1,1,1,1,1,1,1,1,1,1,1,1,1,1,
1,1,1,1,1,1,1,1,1,1,1,1,1,1,1,1,1,1,1,1,1,1,1,1,1,1,1,1,1,1,1,1,1,1,1,1,
1,1,1,1,1,1,1,1,1,1,1,1,1,1,1,1,1,1,1,1,1,1,1,1,1,1,1,1,1,1,1,1,1,1,4),
(0.,0.0526254770366344),(11.6163931973417,12.6136148731756,13.6108365490096,
14.6080582248435,15.6052799006775,16.6025015765114,17.5997232523454,18.5969449281793,
19.5941666040133,20.5913882798473,21.5886099556812,22.5858316315152,23.5830533073491,
24.5802749831831,25.577496659017,26.574718334851,27.5719400106849,28.5691616865189,
29.5663833623529,30.5636050381868,31.5608267140208,32.5580483898547,33.5552700656887,
34.5524917415226,35.5497134173566,36.5469350931905,37.5441567690245,38.5413784448584,
39.5386001206924,40.5358217965264,41.5330434723603,42.5302651481943,43.5274868240282,
44.5247084998622,45.5219301756961,46.5191518515301,47.516373527364,48.513595203198,
49.5108168790319,50.5080385548659,51.5052602306999,52.5024819065338,53.4997035823678,
54.4969252582017,55.4941469340357,56.4913686098696,57.4885902857036,58.4858119615375,
59.4830336373715,60.4802553132055,61.4774769890394,62.4746986648734,63.4719203407073,
64.4691420165413,65.4663636923752,66.4635853682092,67.4608070440431,68.4580287198771,
69.455250395711,70.452472071545,71.4496937473789,72.4469154232129,73.4441370990469,
74.4413587748808,75.4385804507148,76.4358021265487,77.4330238023827,78.4302454782166,
79.4274671540506,80.4246888298845,81.4219105057185,82.4191321815525,83.4163538573864,
84.4135755332204,85.4107972090543,86.4080188848883,87.4052405607222,88.4024622365562,
89.3996839123901,90.3969055882241,91.3941272640581,92.391348939892,93.388570615726,
94.3857922915599,95.3830139673939,96.3802356432278,97.3774573190618,98.3746789948957,
99.3719006707297,100.369122346564,101.366344022398,102.363565698232,103.360787374066,
104.358009049899,105.355230725733,106.352452401567,107.349674077401,108.346895753235,
109.344117429069,110.341339104903,111.338560780737,112.335782456571,113.333004132405,
114.330225808239,115.327447484073,116.324669159907,117.321890835741,118.319112511575,
119.316334187409,120.313555863243,121.310777539077,122.307999214911,123.305220890745,
124.302442566579,125.299664242413,126.296885918246,127.29410759408,128.291329269914,
129.288550945748,130.285772621582,131.282994297416,132.28021597325,133.277437649084,
134.274659324918,135.271881000752,136.269102676586,137.26632435242,138.263546028254,
139.260767704088,140.257989379922,141.255211055756,142.25243273159,143.249654407424,
144.246876083258,145.244097759092,146.241319434926,147.23854111076,148.235762786593,
149.232984462427,150.230206138261,151.227427814095,152.224649489929,153.221871165763,
154.219092841597,155.216314517431,156.213536193265,157.210757869099,158.207979544933,
159.205201220767,160.202422896601,161.199644572435,162.196866248269,163.194087924103,
164.191309599937,165.188531275771,166.185752951605,167.182974627439,168.180196303273,
169.177417979107,170.17463965494,171.171861330774,172.169083006608,173.166304682442,
174.163526358276,175.16074803411,176.157969709944,177.155191385778,178.152413061612,
179.149634737446,180.14685641328,181.144078089114,182.141299764948,183.138521440782,
184.135743116616,185.13296479245,186.130186468284,187.127408144118,188.124629819952,
189.121851495786,190.11907317162,191.116294847454,192.113516523288,193.110738199121,
194.107959874955,195.105181550789,196.102403226623,197.099624902457,198.096846578291,
199.094068254125,200.091289929959,201.088511605793,202.085733281627,203.082954957461,
204.080176633295),.UNSPECIFIED.);
#61=B_SPLINE_SURFACE_WITH_KNOTS('',3,3,((#12818,#12819,#12820,#12821,#12822,
#12823,#12824,#12825,#12826,#12827,#12828,#12829,#12830,#12831,#12832,#12833,
#12834,#12835,#12836,#12837,#12838,#12839,#12840,#12841,#12842,#12843,#12844,
#12845,#12846,#12847,#12848,#12849,#12850,#12851,#12852,#12853,#12854,#12855,
#12856,#12857,#12858,#12859,#12860,#12861,#12862,#12863,#12864,#12865,#12866,
#12867,#12868,#12869,#12870,#12871,#12872,#12873,#12874,#12875,#12876,#12877,
#12878,#12879,#12880,#12881,#12882,#12883,#12884,#12885,#12886,#12887,#12888,
#12889,#12890,#12891,#12892,#12893,#12894,#12895,#12896,#12897,#12898,#12899,
#12900,#12901,#12902,#12903,#12904,#12905,#12906,#12907,#12908,#12909,#12910,
#12911,#12912,#12913,#12914,#12915,#12916,#12917,#12918,#12919,#12920,#12921,
#12922,#12923,#12924,#12925,#12926,#12927,#12928,#12929,#12930,#12931,#12932,
#12933,#12934,#12935,#12936,#12937,#12938,#12939,#12940,#12941,#12942,#12943,
#12944,#12945,#12946,#12947,#12948,#12949,#12950,#12951,#12952,#12953,#12954,
#12955,#12956,#12957,#12958,#12959,#12960,#12961,#12962,#12963,#12964,#12965,
#12966,#12967,#12968,#12969,#12970,#12971,#12972,#12973,#12974,#12975,#12976,
#12977,#12978,#12979,#12980,#12981,#12982,#12983,#12984,#12985,#12986,#12987,
#12988,#12989,#12990,#12991,#12992,#12993,#12994,#12995,#12996,#12997,#12998,
#12999,#13000,#13001,#13002,#13003,#13004,#13005,#13006,#13007,#13008,#13009,
#13010,#13011,#13012,#13013,#13014,#13015),(#13016,#13017,#13018,#13019,
#13020,#13021,#13022,#13023,#13024,#13025,#13026,#13027,#13028,#13029,#13030,
#13031,#13032,#13033,#13034,#13035,#13036,#13037,#13038,#13039,#13040,#13041,
#13042,#13043,#13044,#13045,#13046,#13047,#13048,#13049,#13050,#13051,#13052,
#13053,#13054,#13055,#13056,#13057,#13058,#13059,#13060,#13061,#13062,#13063,
#13064,#13065,#13066,#13067,#13068,#13069,#13070,#13071,#13072,#13073,#13074,
#13075,#13076,#13077,#13078,#13079,#13080,#13081,#13082,#13083,#13084,#13085,
#13086,#13087,#13088,#13089,#13090,#13091,#13092,#13093,#13094,#13095,#13096,
#13097,#13098,#13099,#13100,#13101,#13102,#13103,#13104,#13105,#13106,#13107,
#13108,#13109,#13110,#13111,#13112,#13113,#13114,#13115,#13116,#13117,#13118,
#13119,#13120,#13121,#13122,#13123,#13124,#13125,#13126,#13127,#13128,#13129,
#13130,#13131,#13132,#13133,#13134,#13135,#13136,#13137,#13138,#13139,#13140,
#13141,#13142,#13143,#13144,#13145,#13146,#13147,#13148,#13149,#13150,#13151,
#13152,#13153,#13154,#13155,#13156,#13157,#13158,#13159,#13160,#13161,#13162,
#13163,#13164,#13165,#13166,#13167,#13168,#13169,#13170,#13171,#13172,#13173,
#13174,#13175,#13176,#13177,#13178,#13179,#13180,#13181,#13182,#13183,#13184,
#13185,#13186,#13187,#13188,#13189,#13190,#13191,#13192,#13193,#13194,#13195,
#13196,#13197,#13198,#13199,#13200,#13201,#13202,#13203,#13204,#13205,#13206,
#13207,#13208,#13209,#13210,#13211,#13212,#13213),(#13214,#13215,#13216,
#13217,#13218,#13219,#13220,#13221,#13222,#13223,#13224,#13225,#13226,#13227,
#13228,#13229,#13230,#13231,#13232,#13233,#13234,#13235,#13236,#13237,#13238,
#13239,#13240,#13241,#13242,#13243,#13244,#13245,#13246,#13247,#13248,#13249,
#13250,#13251,#13252,#13253,#13254,#13255,#13256,#13257,#13258,#13259,#13260,
#13261,#13262,#13263,#13264,#13265,#13266,#13267,#13268,#13269,#13270,#13271,
#13272,#13273,#13274,#13275,#13276,#13277,#13278,#13279,#13280,#13281,#13282,
#13283,#13284,#13285,#13286,#13287,#13288,#13289,#13290,#13291,#13292,#13293,
#13294,#13295,#13296,#13297,#13298,#13299,#13300,#13301,#13302,#13303,#13304,
#13305,#13306,#13307,#13308,#13309,#13310,#13311,#13312,#13313,#13314,#13315,
#13316,#13317,#13318,#13319,#13320,#13321,#13322,#13323,#13324,#13325,#13326,
#13327,#13328,#13329,#13330,#13331,#13332,#13333,#13334,#13335,#13336,#13337,
#13338,#13339,#13340,#13341,#13342,#13343,#13344,#13345,#13346,#13347,#13348,
#13349,#13350,#13351,#13352,#13353,#13354,#13355,#13356,#13357,#13358,#13359,
#13360,#13361,#13362,#13363,#13364,#13365,#13366,#13367,#13368,#13369,#13370,
#13371,#13372,#13373,#13374,#13375,#13376,#13377,#13378,#13379,#13380,#13381,
#13382,#13383,#13384,#13385,#13386,#13387,#13388,#13389,#13390,#13391,#13392,
#13393,#13394,#13395,#13396,#13397,#13398,#13399,#13400,#13401,#13402,#13403,
#13404,#13405,#13406,#13407,#13408,#13409,#13410,#13411),(#13412,#13413,
#13414,#13415,#13416,#13417,#13418,#13419,#13420,#13421,#13422,#13423,#13424,
#13425,#13426,#13427,#13428,#13429,#13430,#13431,#13432,#13433,#13434,#13435,
#13436,#13437,#13438,#13439,#13440,#13441,#13442,#13443,#13444,#13445,#13446,
#13447,#13448,#13449,#13450,#13451,#13452,#13453,#13454,#13455,#13456,#13457,
#13458,#13459,#13460,#13461,#13462,#13463,#13464,#13465,#13466,#13467,#13468,
#13469,#13470,#13471,#13472,#13473,#13474,#13475,#13476,#13477,#13478,#13479,
#13480,#13481,#13482,#13483,#13484,#13485,#13486,#13487,#13488,#13489,#13490,
#13491,#13492,#13493,#13494,#13495,#13496,#13497,#13498,#13499,#13500,#13501,
#13502,#13503,#13504,#13505,#13506,#13507,#13508,#13509,#13510,#13511,#13512,
#13513,#13514,#13515,#13516,#13517,#13518,#13519,#13520,#13521,#13522,#13523,
#13524,#13525,#13526,#13527,#13528,#13529,#13530,#13531,#13532,#13533,#13534,
#13535,#13536,#13537,#13538,#13539,#13540,#13541,#13542,#13543,#13544,#13545,
#13546,#13547,#13548,#13549,#13550,#13551,#13552,#13553,#13554,#13555,#13556,
#13557,#13558,#13559,#13560,#13561,#13562,#13563,#13564,#13565,#13566,#13567,
#13568,#13569,#13570,#13571,#13572,#13573,#13574,#13575,#13576,#13577,#13578,
#13579,#13580,#13581,#13582,#13583,#13584,#13585,#13586,#13587,#13588,#13589,
#13590,#13591,#13592,#13593,#13594,#13595,#13596,#13597,#13598,#13599,#13600,
#13601,#13602,#13603,#13604,#13605,#13606,#13607,#13608,#13609)),
 .UNSPECIFIED.,.F.,.F.,.F.,(4,4),(4,1,1,1,1,1,1,1,1,1,1,1,1,1,1,1,1,1,1,
1,1,1,1,1,1,1,1,1,1,1,1,1,1,1,1,1,1,1,1,1,1,1,1,1,1,1,1,1,1,1,1,1,1,1,1,
1,1,1,1,1,1,1,1,1,1,1,1,1,1,1,1,1,1,1,1,1,1,1,1,1,1,1,1,1,1,1,1,1,1,1,1,
1,1,1,1,1,1,1,1,1,1,1,1,1,1,1,1,1,1,1,1,1,1,1,1,1,1,1,1,1,1,1,1,1,1,1,1,
1,1,1,1,1,1,1,1,1,1,1,1,1,1,1,1,1,1,1,1,1,1,1,1,1,1,1,1,1,1,1,1,1,1,1,1,
1,1,1,1,1,1,1,1,1,1,1,1,1,1,1,1,1,1,1,1,1,1,1,1,1,1,1,1,1,1,1,1,4),(0.,
0.0526254770366344),(8.30815772716282,9.3057494250427,10.3033411229226,
11.3009328208025,12.2985245186824,13.2961162165622,14.2937079144421,15.291299612322,
16.2888913102019,17.2864830080818,18.2840747059617,19.2816664038415,20.2792581017214,
21.2768497996013,22.2744414974812,23.2720331953611,24.269624893241,25.2672165911209,
26.2648082890007,27.2623999868806,28.2599916847605,29.2575833826404,30.2551750805203,
31.2527667784002,32.2503584762801,33.2479501741599,34.2455418720398,35.2431335699197,
36.2407252677996,37.2383169656795,38.2359086635594,39.2335003614392,40.2310920593191,
41.228683757199,42.2262754550789,43.2238671529588,44.2214588508387,45.2190505487186,
46.2166422465984,47.2142339444783,48.2118256423582,49.2094173402381,50.207009038118,
51.2046007359979,52.2021924338777,53.1997841317576,54.1973758296375,55.1949675275174,
56.1925592253973,57.1901509232772,58.1877426211571,59.1853343190369,60.1829260169168,
61.1805177147967,62.1781094126766,63.1757011105565,64.1732928084364,65.1708845063163,
66.1684762041961,67.166067902076,68.1636595999559,69.1612512978358,70.1588429957157,
71.1564346935956,72.1540263914755,73.1516180893553,74.1492097872352,75.1468014851151,
76.144393182995,77.1419848808749,78.1395765787548,79.1371682766347,80.1347599745145,
81.1323516723944,82.1299433702743,83.1275350681542,84.1251267660341,85.122718463914,
86.1203101617938,87.1179018596737,88.1154935575536,89.1130852554335,90.1106769533134,
91.1082686511933,92.1058603490732,93.103452046953,94.1010437448329,95.0986354427128,
96.0962271405927,97.0938188384726,98.0914105363525,99.0890022342324,100.086593932112,
101.084185629992,102.081777327872,103.079369025752,104.076960723632,105.074552421512,
106.072144119392,107.069735817271,108.067327515151,109.064919213031,110.062510910911,
111.060102608791,112.057694306671,113.055286004551,114.052877702431,115.050469400311,
116.04806109819,117.04565279607,118.04324449395,119.04083619183,120.03842788971,
121.03601958759,122.03361128547,123.03120298335,124.028794681229,125.026386379109,
126.023978076989,127.021569774869,128.019161472749,129.016753170629,130.014344868509,
131.011936566389,132.009528264269,133.007119962148,134.004711660028,135.002303357908,
135.999895055788,136.997486753668,137.995078451548,138.992670149428,139.990261847308,
140.987853545188,141.985445243067,142.983036940947,143.980628638827,144.978220336707,
145.975812034587,146.973403732467,147.970995430347,148.968587128227,149.966178826106,
150.963770523986,151.961362221866,152.958953919746,153.956545617626,154.954137315506,
155.951729013386,156.949320711266,157.946912409146,158.944504107025,159.942095804905,
160.939687502785,161.937279200665,162.934870898545,163.932462596425,164.930054294305,
165.927645992185,166.925237690065,167.922829387944,168.920421085824,169.918012783704,
170.915604481584,171.913196179464,172.910787877344,173.908379575224,174.905971273104,
175.903562970983,176.901154668863,177.898746366743,178.896338064623,179.893929762503,
180.891521460383,181.889113158263,182.886704856143,183.884296554023,184.881888251902,
185.879479949782,186.877071647662,187.874663345542,188.872255043422,189.869846741302,
190.867438439182,191.865030137062,192.862621834942,193.860213532821,194.857805230701,
195.855396928581,196.852988626461,197.850580324341,198.848172022221,199.845763720101,
200.843355417981,201.84094711586,202.83853881374),.UNSPECIFIED.);
#62=B_SPLINE_CURVE_WITH_KNOTS('',3,(#4900,#4901,#4902,#4903,#4904,#4905,
#4906,#4907,#4908,#4909,#4910,#4911,#4912,#4913,#4914,#4915,#4916,#4917,
#4918),.UNSPECIFIED.,.F.,.F.,(4,3,3,3,3,3,4),(82.9907454093912,83.4361436477206,
84.4294310720982,85.4227184964758,86.4160059208535,87.4092933452311,88.4025807696087),
 .UNSPECIFIED.);
#63=B_SPLINE_CURVE_WITH_KNOTS('',3,(#4922,#4923,#4924,#4925),
 .UNSPECIFIED.,.F.,.F.,(4,4),(-86.3937979737193,-85.5224480267573),
 .UNSPECIFIED.);
#64=B_SPLINE_CURVE_WITH_KNOTS('',3,(#4929,#4930,#4931,#4932,#4933,#4934,
#4935,#4936,#4937,#4938,#4939,#4940,#4941,#4942,#4943,#4944,#4945,#4946,
#4947,#4948,#4949,#4950,#4951,#4952,#4953),.UNSPECIFIED.,.F.,.F.,(4,3,3,
3,3,3,3,3,4),(-85.5224480267573,-85.4227184964758,-84.4294310720982,-83.4361436477206,
-82.442856223343,-81.4495687989653,-80.4562813745877,-79.4629939502101,
-79.2392627195777),.UNSPECIFIED.);
#65=B_SPLINE_CURVE_WITH_KNOTS('',3,(#4958,#4959,#4960,#4961,#4962,#4963,
#4964,#4965,#4966,#4967,#4968,#4969,#4970,#4971,#4972,#4973,#4974,#4975,
#4976,#4977,#4978,#4979),.UNSPECIFIED.,.F.,.F.,(4,3,3,3,3,3,3,4),(76.7075601022116,
77.4764191014548,78.4697065258324,79.4629939502101,80.4562813745877,81.4495687989653,
82.442856223343,82.9907454093912),.UNSPECIFIED.);
#66=B_SPLINE_CURVE_WITH_KNOTS('',3,(#4980,#4981,#4982,#4983,#4984,#4985,
#4986,#4987,#4988,#4989,#4990,#4991,#4992,#4993,#4994,#4995,#4996,#4997,
#4998,#4999,#5000,#5001),.UNSPECIFIED.,.F.,.F.,(4,3,3,3,3,3,3,4),(-79.2392627195777,
-78.4697065258324,-77.4764191014548,-76.4831316770772,-75.4898442526996,
-74.4965568283219,-73.5032694039443,-72.9560774123981),.UNSPECIFIED.);
#67=B_SPLINE_CURVE_WITH_KNOTS('',3,(#5006,#5007,#5008,#5009,#5010,#5011,
#5012,#5013,#5014,#5015,#5016,#5017,#5018,#5019,#5020,#5021,#5022,#5023,
#5024,#5025,#5026,#5027,#5028,#5029,#5030),.UNSPECIFIED.,.F.,.F.,(4,3,3,
3,3,3,3,3,4),(70.424374795032,70.5234071308114,71.516694555189,72.5099819795667,
73.5032694039443,74.4965568283219,75.4898442526996,76.4831316770772,76.7075601022116),
 .UNSPECIFIED.);
#68=B_SPLINE_CURVE_WITH_KNOTS('',3,(#5031,#5032,#5033,#5034,#5035,#5036,
#5037,#5038,#5039,#5040,#5041,#5042,#5043,#5044,#5045,#5046,#5047,#5048,
#5049,#5050,#5051,#5052),.UNSPECIFIED.,.F.,.F.,(4,3,3,3,3,3,3,4),(-72.9560774123981,
-72.5099819795667,-71.516694555189,-70.5234071308114,-69.5301197064338,
-68.5368322820562,-67.5435448576786,-66.6728921052185),.UNSPECIFIED.);
#69=B_SPLINE_CURVE_WITH_KNOTS('',3,(#5057,#5058,#5059,#5060,#5061,#5062,
#5063,#5064,#5065,#5066,#5067,#5068,#5069,#5070,#5071,#5072,#5073,#5074,
#5075,#5076,#5077,#5078),.UNSPECIFIED.,.F.,.F.,(4,3,3,3,3,3,3,4),(64.1411894878524,
64.5636825845457,65.5569700089233,66.5502574333009,67.5435448576786,68.5368322820562,
69.5301197064338,70.424374795032),.UNSPECIFIED.);
#70=B_SPLINE_CURVE_WITH_KNOTS('',3,(#5079,#5080,#5081,#5082,#5083,#5084,
#5085,#5086,#5087,#5088,#5089,#5090,#5091,#5092,#5093,#5094,#5095,#5096,
#5097,#5098,#5099,#5100,#5101,#5102,#5103),.UNSPECIFIED.,.F.,.F.,(4,3,3,
3,3,3,3,3,4),(-66.6728921052185,-66.550257433301,-65.5569700089233,-64.5636825845457,
-63.5703951601681,-62.5771077357904,-61.5838203114128,-60.5905328870352,
-60.3897067980389),.UNSPECIFIED.);
#71=B_SPLINE_CURVE_WITH_KNOTS('',3,(#5108,#5109,#5110,#5111,#5112,#5113,
#5114,#5115,#5116,#5117,#5118,#5119,#5120,#5121,#5122,#5123,#5124,#5125,
#5126,#5127,#5128,#5129),.UNSPECIFIED.,.F.,.F.,(4,3,3,3,3,3,3,4),(57.8580041806728,
58.6039580382799,59.5972454626575,60.5905328870352,61.5838203114128,62.5771077357904,
63.570395160168,64.1411894878524),.UNSPECIFIED.);
#72=B_SPLINE_CURVE_WITH_KNOTS('',3,(#5130,#5131,#5132,#5133,#5134,#5135,
#5136,#5137,#5138,#5139,#5140,#5141,#5142,#5143,#5144,#5145,#5146,#5147,
#5148,#5149,#5150,#5151),.UNSPECIFIED.,.F.,.F.,(4,3,3,3,3,3,3,4),(-60.3897067980389,
-59.5972454626576,-58.6039580382799,-57.6106706139023,-56.6173831895247,
-55.624095765147,-54.6308083407694,-54.1065214908593),.UNSPECIFIED.);
#73=B_SPLINE_CURVE_WITH_KNOTS('',3,(#5156,#5157,#5158,#5159,#5160,#5161,
#5162,#5163,#5164,#5165,#5166,#5167,#5168,#5169,#5170,#5171,#5172,#5173,
#5174,#5175,#5176,#5177,#5178,#5179,#5180),.UNSPECIFIED.,.F.,.F.,(4,3,3,
3,3,3,3,3,4),(51.5748188734932,51.6509460676365,52.6442334920142,53.6375209163918,
54.6308083407694,55.624095765147,56.6173831895247,57.6106706139023,57.8580041806728),
 .UNSPECIFIED.);
#74=B_SPLINE_CURVE_WITH_KNOTS('',3,(#5181,#5182,#5183,#5184,#5185,#5186,
#5187,#5188,#5189,#5190,#5191,#5192,#5193,#5194,#5195,#5196,#5197,#5198,
#5199,#5200,#5201,#5202),.UNSPECIFIED.,.F.,.F.,(4,3,3,3,3,3,3,4),(-54.1065214908593,
-53.6375209163918,-52.6442334920142,-51.6509460676365,-50.6576586432589,
-49.6643712188813,-48.6710837945037,-47.8233361836797),.UNSPECIFIED.);
#75=B_SPLINE_CURVE_WITH_KNOTS('',3,(#5207,#5208,#5209,#5210,#5211,#5212,
#5213,#5214,#5215,#5216,#5217,#5218,#5219,#5220,#5221,#5222,#5223,#5224,
#5225,#5226,#5227,#5228),.UNSPECIFIED.,.F.,.F.,(4,3,3,3,3,3,3,4),(45.2916335663136,
45.6912215213708,46.6845089457484,47.677796370126,48.6710837945037,49.6643712188813,
50.6576586432589,51.5748188734932),.UNSPECIFIED.);
#76=B_SPLINE_CURVE_WITH_KNOTS('',3,(#5229,#5230,#5231,#5232,#5233,#5234,
#5235,#5236,#5237,#5238,#5239,#5240,#5241,#5242,#5243,#5244,#5245,#5246,
#5247,#5248,#5249,#5250,#5251,#5252,#5253),.UNSPECIFIED.,.F.,.F.,(4,3,3,
3,3,3,3,3,4),(-47.8233361836797,-47.677796370126,-46.6845089457484,-45.6912215213708,
-44.6979340969932,-43.7046466726155,-42.7113592482379,-41.7180718238603,
-41.5401508765001),.UNSPECIFIED.);
#77=B_SPLINE_CURVE_WITH_KNOTS('',3,(#5258,#5259,#5260,#5261,#5262,#5263,
#5264,#5265,#5266,#5267,#5268,#5269,#5270,#5271,#5272,#5273,#5274,#5275,
#5276,#5277,#5278,#5279),.UNSPECIFIED.,.F.,.F.,(4,3,3,3,3,3,3,4),(39.008448259134,
39.731496975105,40.7247843994827,41.7180718238603,42.7113592482379,43.7046466726155,
44.6979340969932,45.2916335663136),.UNSPECIFIED.);
#78=B_SPLINE_CURVE_WITH_KNOTS('',3,(#5280,#5281,#5282,#5283,#5284,#5285,
#5286,#5287,#5288,#5289,#5290,#5291,#5292,#5293,#5294,#5295,#5296,#5297,
#5298,#5299,#5300,#5301),.UNSPECIFIED.,.F.,.F.,(4,3,3,3,3,3,3,4),(-41.5401508765001,
-40.7247843994827,-39.731496975105,-38.7382095507274,-37.7449221263498,
-36.7516347019722,-35.7583472775945,-35.2569655693205),.UNSPECIFIED.);
#79=B_SPLINE_CURVE_WITH_KNOTS('',3,(#5306,#5307,#5308,#5309,#5310,#5311,
#5312,#5313,#5314,#5315,#5316,#5317,#5318,#5319,#5320,#5321,#5322,#5323,
#5324,#5325,#5326,#5327,#5328,#5329,#5330),.UNSPECIFIED.,.F.,.F.,(4,3,3,
3,3,3,3,3,4),(32.7252629519544,32.7784850044617,33.7717724288393,34.7650598532169,
35.7583472775945,36.7516347019722,37.7449221263498,38.7382095507274,39.008448259134),
 .UNSPECIFIED.);
#80=B_SPLINE_CURVE_WITH_KNOTS('',3,(#5331,#5332,#5333,#5334,#5335,#5336,
#5337,#5338,#5339,#5340,#5341,#5342,#5343,#5344,#5345,#5346,#5347,#5348,
#5349,#5350,#5351,#5352),.UNSPECIFIED.,.F.,.F.,(4,3,3,3,3,3,3,4),(-35.2569655693205,
-34.7650598532169,-33.7717724288393,-32.7784850044617,-31.785197580084,
-30.7919101557064,-29.7986227313288,-28.973780262141),.UNSPECIFIED.);
#81=B_SPLINE_CURVE_WITH_KNOTS('',3,(#5357,#5358,#5359,#5360,#5361,#5362,
#5363,#5364,#5365,#5366,#5367,#5368,#5369,#5370,#5371,#5372,#5373,#5374,
#5375,#5376,#5377,#5378),.UNSPECIFIED.,.F.,.F.,(4,3,3,3,3,3,3,4),(26.4420776447749,
26.8187604581959,27.8120478825735,28.8053353069512,29.7986227313288,30.7919101557064,
31.785197580084,32.7252629519544),.UNSPECIFIED.);
#82=B_SPLINE_CURVE_WITH_KNOTS('',3,(#5379,#5380,#5381,#5382,#5383,#5384,
#5385,#5386,#5387,#5388,#5389,#5390,#5391,#5392,#5393,#5394,#5395,#5396,
#5397,#5398,#5399,#5400,#5401,#5402,#5403),.UNSPECIFIED.,.F.,.F.,(4,3,3,
3,3,3,3,3,4),(-28.973780262141,-28.8053353069512,-27.8120478825735,-26.8187604581959,
-25.8254730338183,-24.8321856094406,-23.838898185063,-22.8456107606854,
-22.6905949549614),.UNSPECIFIED.);
#83=B_SPLINE_CURVE_WITH_KNOTS('',3,(#5408,#5409,#5410,#5411,#5412,#5413,
#5414,#5415,#5416,#5417,#5418,#5419,#5420,#5421,#5422,#5423,#5424,#5425,
#5426,#5427,#5428,#5429),.UNSPECIFIED.,.F.,.F.,(4,3,3,3,3,3,3,4),(20.1588923375953,
20.8590359119301,21.8523233363078,22.8456107606854,23.838898185063,24.8321856094406,
25.8254730338183,26.4420776447749),.UNSPECIFIED.);
#84=B_SPLINE_CURVE_WITH_KNOTS('',3,(#5430,#5431,#5432,#5433,#5434,#5435,
#5436,#5437,#5438,#5439,#5440,#5441,#5442,#5443,#5444,#5445,#5446,#5447,
#5448,#5449,#5450,#5451),.UNSPECIFIED.,.F.,.F.,(4,3,3,3,3,3,3,4),(-22.6905949549614,
-21.8523233363078,-20.8590359119301,-19.8657484875525,-18.8724610631749,
-17.8791736387973,-16.8858862144196,-16.4074096477818),.UNSPECIFIED.);
#85=B_SPLINE_CURVE_WITH_KNOTS('',3,(#5456,#5457,#5458,#5459,#5460,#5461,
#5462,#5463,#5464,#5465,#5466,#5467,#5468,#5469,#5470,#5471,#5472,#5473,
#5474,#5475,#5476,#5477,#5478,#5479,#5480),.UNSPECIFIED.,.F.,.F.,(4,3,3,
3,3,3,3,3,4),(13.8757070304157,13.9060239412868,14.8993113656644,15.892598790042,
16.8858862144196,17.8791736387973,18.8724610631749,19.8657484875525,20.1588923375953),
 .UNSPECIFIED.);
#86=B_SPLINE_CURVE_WITH_KNOTS('',3,(#5481,#5482,#5483,#5484,#5485,#5486,
#5487,#5488,#5489,#5490,#5491,#5492,#5493,#5494,#5495,#5496,#5497,#5498,
#5499,#5500,#5501,#5502),.UNSPECIFIED.,.F.,.F.,(4,3,3,3,3,3,3,4),(-16.4074096477818,
-15.892598790042,-14.8993113656644,-13.9060239412868,-12.9127365169091,
-11.9194490925315,-10.9261616681539,-10.1242243406022),.UNSPECIFIED.);
#87=B_SPLINE_CURVE_WITH_KNOTS('',3,(#5508,#5509,#5510,#5511,#5512,#5513,
#5514,#5515,#5516,#5517,#5518,#5519,#5520),.UNSPECIFIED.,.F.,.F.,(4,3,3,
3,4),(-3.84103903342261,-2.97986227313288,-1.98657484875525,-0.993287424377625,
0.),.UNSPECIFIED.);
#88=B_SPLINE_CURVE_WITH_KNOTS('',3,(#5523,#5524,#5525,#5526,#5527,#5528,
#5529,#5530,#5531,#5532,#5533,#5534,#5535,#5536,#5537,#5538,#5539,#5540,
#5541),.UNSPECIFIED.,.F.,.F.,(4,3,3,3,3,3,4),(2.00878279588941,2.97986227313288,
3.9731496975105,4.96643712188813,5.95972454626575,6.95301197064338,7.5925217232361),
 .UNSPECIFIED.);
#89=B_SPLINE_CURVE_WITH_KNOTS('',3,(#5547,#5548,#5549,#5550,#5551,#5552),
 .UNSPECIFIED.,.F.,.F.,(4,1,1,4),(97.3893722612836,98.2829301553797,99.2762175797573,
100.269505004135),.UNSPECIFIED.);
#90=B_SPLINE_CURVE_WITH_KNOTS('',3,(#5555,#5556,#5557,#5558,#5559,#5560,
#5561),.UNSPECIFIED.,.F.,.F.,(4,1,1,1,4),(97.3893722612836,97.8347704996129,
98.8280579239905,99.8213453483681,100.792424825612),.UNSPECIFIED.);
#91=B_SPLINE_CURVE_WITH_KNOTS('',3,(#5566,#5567,#5568,#5569,#5570,#5571,
#5572,#5573,#5574,#5575,#5576),.UNSPECIFIED.,.F.,.F.,(4,1,1,1,1,1,1,1,4),
(91.106186954104,91.3299181847363,92.323205609114,93.3164930334916,94.3097804578692,
95.3030678822468,96.2963553066245,97.2896427310021,97.3893722612836),
 .UNSPECIFIED.);
#92=B_SPLINE_CURVE_WITH_KNOTS('',3,(#5577,#5578,#5579,#5580,#5581,#5582,
#5583,#5584,#5585,#5586),.UNSPECIFIED.,.F.,.F.,(4,1,1,1,1,1,1,4),(91.106186954104,
91.8750459533471,92.8683333777248,93.8616208021024,94.85490822648,95.8481956508576,
96.8414830752353,97.3893722612836),.UNSPECIFIED.);
#93=B_SPLINE_CURVE_WITH_KNOTS('',3,(#5591,#5592,#5593,#5594,#5595,#5596,
#5597,#5598,#5599,#5600),.UNSPECIFIED.,.F.,.F.,(4,1,1,1,1,1,1,4),(84.8230016469244,
85.3701936384706,86.3634810628482,87.3567684872258,88.3500559116035,89.3433433359811,
90.3366307603587,91.106186954104),.UNSPECIFIED.);
#94=B_SPLINE_CURVE_WITH_KNOTS('',3,(#5601,#5602,#5603,#5604,#5605,#5606,
#5607,#5608,#5609,#5610,#5611),.UNSPECIFIED.,.F.,.F.,(4,1,1,1,1,1,1,1,4),
(84.8230016469244,84.9220339827037,85.9153214070814,86.908608831459,87.9018962558366,
88.8951836802142,89.8884711045919,90.8817585289695,91.106186954104),
 .UNSPECIFIED.);
#95=B_SPLINE_CURVE_WITH_KNOTS('',3,(#5616,#5617,#5618,#5619,#5620,#5621,
#5622,#5623,#5624,#5625),.UNSPECIFIED.,.F.,.F.,(4,1,1,1,1,1,1,4),(78.5398163397448,
79.4104690922048,80.4037565165825,81.3970439409601,82.3903313653377,83.3836187897153,
84.376906214093,84.8230016469244),.UNSPECIFIED.);
#96=B_SPLINE_CURVE_WITH_KNOTS('',3,(#5626,#5627,#5628,#5629,#5630,#5631,
#5632,#5633,#5634,#5635),.UNSPECIFIED.,.F.,.F.,(4,1,1,1,1,1,1,4),(78.5398163397448,
78.962309436438,79.9555968608156,80.9488842851932,81.9421717095709,82.9354591339485,
83.9287465583261,84.8230016469244),.UNSPECIFIED.);
#97=B_SPLINE_CURVE_WITH_KNOTS('',3,(#5640,#5641,#5642,#5643,#5644,#5645,
#5646,#5647,#5648,#5649,#5650),.UNSPECIFIED.,.F.,.F.,(4,1,1,1,1,1,1,1,4),
(72.2566310325652,72.4574571215614,73.4507445459391,74.4440319703167,75.4373193946943,
76.430606819072,77.4238942434496,78.4171816678272,78.5398163397448),
 .UNSPECIFIED.);
#98=B_SPLINE_CURVE_WITH_KNOTS('',3,(#5651,#5652,#5653,#5654,#5655,#5656,
#5657,#5658,#5659,#5660),.UNSPECIFIED.,.F.,.F.,(4,1,1,1,1,1,1,4),(72.2566310325652,
73.0025848901722,73.9958723145499,74.9891597389275,75.9824471633051,76.9757345876827,
77.9690220120604,78.5398163397448),.UNSPECIFIED.);
#99=B_SPLINE_CURVE_WITH_KNOTS('',3,(#5665,#5666,#5667,#5668,#5669,#5670,
#5671,#5672,#5673,#5674),.UNSPECIFIED.,.F.,.F.,(4,1,1,1,1,1,1,4),(65.9734457253856,
66.4977325752957,67.4910199996733,68.4843074240509,69.4775948484286,70.4708822728062,
71.4641696971838,72.2566310325652),.UNSPECIFIED.);
#100=B_SPLINE_CURVE_WITH_KNOTS('',3,(#5675,#5676,#5677,#5678,#5679,#5680,
#5681,#5682,#5683,#5684,#5685),.UNSPECIFIED.,.F.,.F.,(4,1,1,1,1,1,1,1,4),
(65.9734457253856,66.0495729195289,67.0428603439065,68.0361477682841,69.0294351926617,
70.0227226170393,71.016010041417,72.0092974657946,72.2566310325652),
 .UNSPECIFIED.);
#101=B_SPLINE_CURVE_WITH_KNOTS('',3,(#5690,#5691,#5692,#5693,#5694,#5695,
#5696,#5697,#5698,#5699),.UNSPECIFIED.,.F.,.F.,(4,1,1,1,1,1,1,4),(59.690260418206,
60.5380080290299,61.5312954534076,62.5245828777852,63.5178703021628,64.5111577265404,
65.5044451509181,65.9734457253856),.UNSPECIFIED.);
#102=B_SPLINE_CURVE_WITH_KNOTS('',3,(#5700,#5701,#5702,#5703,#5704,#5705,
#5706,#5707,#5708,#5709),.UNSPECIFIED.,.F.,.F.,(4,1,1,1,1,1,1,4),(59.690260418206,
60.0898483732631,61.0831357976407,62.0764232220183,63.069710646396,64.0629980707736,
65.0562854951512,65.9734457253856),.UNSPECIFIED.);
#103=B_SPLINE_CURVE_WITH_KNOTS('',3,(#5714,#5715,#5716,#5717,#5718,#5719,
#5720,#5721,#5722,#5723,#5724),.UNSPECIFIED.,.F.,.F.,(4,1,1,1,1,1,1,1,4),
(53.4070751110264,53.5849960583866,54.5782834827642,55.5715709071418,56.5648583315194,
57.5581457558971,58.5514331802747,59.5447206046523,59.690260418206),
 .UNSPECIFIED.);
#104=B_SPLINE_CURVE_WITH_KNOTS('',3,(#5725,#5726,#5727,#5728,#5729,#5730,
#5731,#5732,#5733,#5734),.UNSPECIFIED.,.F.,.F.,(4,1,1,1,1,1,1,4),(53.4070751110264,
54.1301238269973,55.123411251375,56.1166986757526,57.1099861001302,58.1032735245078,
59.0965609488855,59.690260418206),.UNSPECIFIED.);
#105=B_SPLINE_CURVE_WITH_KNOTS('',3,(#5739,#5740,#5741,#5742,#5743,#5744,
#5745,#5746,#5747,#5748),.UNSPECIFIED.,.F.,.F.,(4,1,1,1,1,1,1,4),(47.1238898038468,
47.6252715121208,48.6185589364984,49.6118463608761,50.6051337852537,51.5984212096313,
52.5917086340089,53.4070751110264),.UNSPECIFIED.);
#106=B_SPLINE_CURVE_WITH_KNOTS('',3,(#5749,#5750,#5751,#5752,#5753,#5754,
#5755,#5756,#5757,#5758,#5759),.UNSPECIFIED.,.F.,.F.,(4,1,1,1,1,1,1,1,4),
(47.1238898038468,47.177111856354,48.1703992807316,49.1636867051092,50.1569741294868,
51.1502615538645,52.1435489782421,53.1368364026197,53.4070751110264),
 .UNSPECIFIED.);
#107=B_SPLINE_CURVE_WITH_KNOTS('',3,(#5764,#5765,#5766,#5767,#5768,#5769,
#5770,#5771,#5772,#5773),.UNSPECIFIED.,.F.,.F.,(4,1,1,1,1,1,1,4),(40.8407044966673,
41.6655469658551,42.6588343902327,43.6521218146103,44.6454092389879,45.6386966633656,
46.6319840877432,47.1238898038468),.UNSPECIFIED.);
#108=B_SPLINE_CURVE_WITH_KNOTS('',3,(#5774,#5775,#5776,#5777,#5778,#5779,
#5780,#5781,#5782,#5783),.UNSPECIFIED.,.F.,.F.,(4,1,1,1,1,1,1,4),(40.8407044966672,
41.2173873100882,42.2106747344658,43.2039621588435,44.1972495832211,45.1905370075987,
46.1838244319763,47.1238898038468),.UNSPECIFIED.);
#109=B_SPLINE_CURVE_WITH_KNOTS('',3,(#5788,#5789,#5790,#5791,#5792,#5793,
#5794,#5795,#5796,#5797,#5798),.UNSPECIFIED.,.F.,.F.,(4,1,1,1,1,1,1,1,4),
(34.5575191894876,34.7125349952117,35.7058224195893,36.6991098439669,37.6923972683445,
38.6856846927222,39.6789721170998,40.6722595414774,40.8407044966673),
 .UNSPECIFIED.);
#110=B_SPLINE_CURVE_WITH_KNOTS('',3,(#5799,#5800,#5801,#5802,#5803,#5804,
#5805,#5806,#5807,#5808),.UNSPECIFIED.,.F.,.F.,(4,1,1,1,1,1,1,4),(34.5575191894876,
35.2576627638225,36.2509501882001,37.2442376125777,38.2375250369553,39.230812461333,
40.2240998857106,40.8407044966672),.UNSPECIFIED.);
#111=B_SPLINE_CURVE_WITH_KNOTS('',3,(#5813,#5814,#5815,#5816,#5817,#5818,
#5819,#5820,#5821,#5822),.UNSPECIFIED.,.F.,.F.,(4,1,1,1,1,1,1,4),(28.2743338823081,
28.7528104489459,29.7460978733235,30.7393852977012,31.7326727220788,32.7259601464564,
33.719247570834,34.5575191894876),.UNSPECIFIED.);
#112=B_SPLINE_CURVE_WITH_KNOTS('',3,(#5823,#5824,#5825,#5826,#5827,#5828,
#5829,#5830,#5831,#5832,#5833),.UNSPECIFIED.,.F.,.F.,(4,1,1,1,1,1,1,1,4),
(28.2743338823081,28.3046507931791,29.2979382175567,30.2912256419343,31.284513066312,
32.2778004906896,33.2710879150672,34.2643753394448,34.5575191894876),
 .UNSPECIFIED.);
#113=B_SPLINE_CURVE_WITH_KNOTS('',3,(#5838,#5839,#5840,#5841,#5842,#5843,
#5844,#5845,#5846,#5847),.UNSPECIFIED.,.F.,.F.,(4,1,1,1,1,1,1,4),(21.9911485751285,
22.7930859026802,23.7863733270578,24.7796607514354,25.772948175813,26.7662356001907,
27.7595230245683,28.2743338823081),.UNSPECIFIED.);
#114=B_SPLINE_CURVE_WITH_KNOTS('',3,(#5848,#5849,#5850,#5851,#5852,#5853,
#5854,#5855,#5856,#5857),.UNSPECIFIED.,.F.,.F.,(4,1,1,1,1,1,1,4),(21.9911485751285,
22.3449262469133,23.3382136712909,24.3315010956686,25.3247885200462,26.3180759444238,
27.3113633688014,28.2743338823081),.UNSPECIFIED.);
#115=B_SPLINE_CURVE_WITH_KNOTS('',3,(#5863,#5864,#5865,#5866,#5867),
 .UNSPECIFIED.,.F.,.F.,(4,1,4),(14.3986268518923,15.3919142762699,15.7079632679489),
 .UNSPECIFIED.);
#116=B_SPLINE_CURVE_WITH_KNOTS('',3,(#5870,#5871,#5872,#5873,#5874),
 .UNSPECIFIED.,.F.,.F.,(4,1,4),(13.8757070304157,14.8467865076592,15.7079632679489),
 .UNSPECIFIED.);
#117=B_SPLINE_CURVE_WITH_KNOTS('',3,(#5880,#5881,#5882,#5883,#5884,#5885,
#5886,#5887,#5888,#5889,#5890,#5891,#5892,#5893,#5894,#5895,#5896,#5897,
#5898),.UNSPECIFIED.,.F.,.F.,(4,3,3,3,3,3,4),(82.9907454093912,83.4361436477206,
84.4294310720982,85.4227184964758,86.4160059208535,87.4092933452311,88.4025807696087),
 .UNSPECIFIED.);
#118=B_SPLINE_CURVE_WITH_KNOTS('',3,(#5902,#5903,#5904,#5905),
 .UNSPECIFIED.,.F.,.F.,(4,4),(-86.3937979737193,-85.5224480267573),
 .UNSPECIFIED.);
#119=B_SPLINE_CURVE_WITH_KNOTS('',3,(#5909,#5910,#5911,#5912,#5913,#5914,
#5915,#5916,#5917,#5918,#5919,#5920,#5921,#5922,#5923,#5924,#5925,#5926,
#5927,#5928,#5929,#5930,#5931,#5932,#5933),.UNSPECIFIED.,.F.,.F.,(4,3,3,
3,3,3,3,3,4),(-85.5224480267573,-85.4227184964758,-84.4294310720982,-83.4361436477206,
-82.442856223343,-81.4495687989653,-80.4562813745877,-79.4629939502101,
-79.2392627195777),.UNSPECIFIED.);
#120=B_SPLINE_CURVE_WITH_KNOTS('',3,(#5938,#5939,#5940,#5941,#5942,#5943,
#5944,#5945,#5946,#5947,#5948,#5949,#5950,#5951,#5952,#5953,#5954,#5955,
#5956,#5957,#5958,#5959),.UNSPECIFIED.,.F.,.F.,(4,3,3,3,3,3,3,4),(76.7075601022116,
77.4764191014548,78.4697065258324,79.4629939502101,80.4562813745877,81.4495687989653,
82.442856223343,82.9907454093912),.UNSPECIFIED.);
#121=B_SPLINE_CURVE_WITH_KNOTS('',3,(#5960,#5961,#5962,#5963,#5964,#5965,
#5966,#5967,#5968,#5969,#5970,#5971,#5972,#5973,#5974,#5975,#5976,#5977,
#5978,#5979,#5980,#5981),.UNSPECIFIED.,.F.,.F.,(4,3,3,3,3,3,3,4),(-79.2392627195777,
-78.4697065258324,-77.4764191014548,-76.4831316770772,-75.4898442526996,
-74.4965568283219,-73.5032694039443,-72.9560774123981),.UNSPECIFIED.);
#122=B_SPLINE_CURVE_WITH_KNOTS('',3,(#5986,#5987,#5988,#5989,#5990,#5991,
#5992,#5993,#5994,#5995,#5996,#5997,#5998,#5999,#6000,#6001,#6002,#6003,
#6004,#6005,#6006,#6007,#6008,#6009,#6010),.UNSPECIFIED.,.F.,.F.,(4,3,3,
3,3,3,3,3,4),(70.424374795032,70.5234071308114,71.516694555189,72.5099819795667,
73.5032694039443,74.4965568283219,75.4898442526996,76.4831316770772,76.7075601022116),
 .UNSPECIFIED.);
#123=B_SPLINE_CURVE_WITH_KNOTS('',3,(#6011,#6012,#6013,#6014,#6015,#6016,
#6017,#6018,#6019,#6020,#6021,#6022,#6023,#6024,#6025,#6026,#6027,#6028,
#6029,#6030,#6031,#6032),.UNSPECIFIED.,.F.,.F.,(4,3,3,3,3,3,3,4),(-72.9560774123981,
-72.5099819795667,-71.516694555189,-70.5234071308114,-69.5301197064338,
-68.5368322820562,-67.5435448576786,-66.6728921052185),.UNSPECIFIED.);
#124=B_SPLINE_CURVE_WITH_KNOTS('',3,(#6037,#6038,#6039,#6040,#6041,#6042,
#6043,#6044,#6045,#6046,#6047,#6048,#6049,#6050,#6051,#6052,#6053,#6054,
#6055,#6056,#6057,#6058),.UNSPECIFIED.,.F.,.F.,(4,3,3,3,3,3,3,4),(64.1411894878524,
64.5636825845457,65.5569700089233,66.5502574333009,67.5435448576786,68.5368322820562,
69.5301197064338,70.424374795032),.UNSPECIFIED.);
#125=B_SPLINE_CURVE_WITH_KNOTS('',3,(#6059,#6060,#6061,#6062,#6063,#6064,
#6065,#6066,#6067,#6068,#6069,#6070,#6071,#6072,#6073,#6074,#6075,#6076,
#6077,#6078,#6079,#6080,#6081,#6082,#6083),.UNSPECIFIED.,.F.,.F.,(4,3,3,
3,3,3,3,3,4),(-66.6728921052185,-66.550257433301,-65.5569700089233,-64.5636825845457,
-63.5703951601681,-62.5771077357904,-61.5838203114128,-60.5905328870352,
-60.3897067980389),.UNSPECIFIED.);
#126=B_SPLINE_CURVE_WITH_KNOTS('',3,(#6088,#6089,#6090,#6091,#6092,#6093,
#6094,#6095,#6096,#6097,#6098,#6099,#6100,#6101,#6102,#6103,#6104,#6105,
#6106,#6107,#6108,#6109),.UNSPECIFIED.,.F.,.F.,(4,3,3,3,3,3,3,4),(57.8580041806728,
58.6039580382799,59.5972454626575,60.5905328870352,61.5838203114128,62.5771077357904,
63.570395160168,64.1411894878524),.UNSPECIFIED.);
#127=B_SPLINE_CURVE_WITH_KNOTS('',3,(#6110,#6111,#6112,#6113,#6114,#6115,
#6116,#6117,#6118,#6119,#6120,#6121,#6122,#6123,#6124,#6125,#6126,#6127,
#6128,#6129,#6130,#6131),.UNSPECIFIED.,.F.,.F.,(4,3,3,3,3,3,3,4),(-60.3897067980389,
-59.5972454626576,-58.6039580382799,-57.6106706139023,-56.6173831895247,
-55.624095765147,-54.6308083407694,-54.1065214908593),.UNSPECIFIED.);
#128=B_SPLINE_CURVE_WITH_KNOTS('',3,(#6136,#6137,#6138,#6139,#6140,#6141,
#6142,#6143,#6144,#6145,#6146,#6147,#6148,#6149,#6150,#6151,#6152,#6153,
#6154,#6155,#6156,#6157,#6158,#6159,#6160),.UNSPECIFIED.,.F.,.F.,(4,3,3,
3,3,3,3,3,4),(51.5748188734932,51.6509460676365,52.6442334920142,53.6375209163918,
54.6308083407694,55.624095765147,56.6173831895247,57.6106706139023,57.8580041806728),
 .UNSPECIFIED.);
#129=B_SPLINE_CURVE_WITH_KNOTS('',3,(#6161,#6162,#6163,#6164,#6165,#6166,
#6167,#6168,#6169,#6170,#6171,#6172,#6173,#6174,#6175,#6176,#6177,#6178,
#6179,#6180,#6181,#6182),.UNSPECIFIED.,.F.,.F.,(4,3,3,3,3,3,3,4),(-54.1065214908593,
-53.6375209163918,-52.6442334920142,-51.6509460676365,-50.6576586432589,
-49.6643712188813,-48.6710837945037,-47.8233361836797),.UNSPECIFIED.);
#130=B_SPLINE_CURVE_WITH_KNOTS('',3,(#6187,#6188,#6189,#6190,#6191,#6192,
#6193,#6194,#6195,#6196,#6197,#6198,#6199,#6200,#6201,#6202,#6203,#6204,
#6205,#6206,#6207,#6208),.UNSPECIFIED.,.F.,.F.,(4,3,3,3,3,3,3,4),(45.2916335663136,
45.6912215213708,46.6845089457484,47.677796370126,48.6710837945037,49.6643712188813,
50.6576586432589,51.5748188734932),.UNSPECIFIED.);
#131=B_SPLINE_CURVE_WITH_KNOTS('',3,(#6209,#6210,#6211,#6212,#6213,#6214,
#6215,#6216,#6217,#6218,#6219,#6220,#6221,#6222,#6223,#6224,#6225,#6226,
#6227,#6228,#6229,#6230,#6231,#6232,#6233),.UNSPECIFIED.,.F.,.F.,(4,3,3,
3,3,3,3,3,4),(-47.8233361836797,-47.677796370126,-46.6845089457484,-45.6912215213708,
-44.6979340969932,-43.7046466726155,-42.7113592482379,-41.7180718238603,
-41.5401508765001),.UNSPECIFIED.);
#132=B_SPLINE_CURVE_WITH_KNOTS('',3,(#6238,#6239,#6240,#6241,#6242,#6243,
#6244,#6245,#6246,#6247,#6248,#6249,#6250,#6251,#6252,#6253,#6254,#6255,
#6256,#6257,#6258,#6259),.UNSPECIFIED.,.F.,.F.,(4,3,3,3,3,3,3,4),(39.008448259134,
39.731496975105,40.7247843994827,41.7180718238603,42.7113592482379,43.7046466726155,
44.6979340969932,45.2916335663136),.UNSPECIFIED.);
#133=B_SPLINE_CURVE_WITH_KNOTS('',3,(#6260,#6261,#6262,#6263,#6264,#6265,
#6266,#6267,#6268,#6269,#6270,#6271,#6272,#6273,#6274,#6275,#6276,#6277,
#6278,#6279,#6280,#6281),.UNSPECIFIED.,.F.,.F.,(4,3,3,3,3,3,3,4),(-41.5401508765001,
-40.7247843994827,-39.731496975105,-38.7382095507274,-37.7449221263498,
-36.7516347019722,-35.7583472775945,-35.2569655693205),.UNSPECIFIED.);
#134=B_SPLINE_CURVE_WITH_KNOTS('',3,(#6286,#6287,#6288,#6289,#6290,#6291,
#6292,#6293,#6294,#6295,#6296,#6297,#6298,#6299,#6300,#6301,#6302,#6303,
#6304,#6305,#6306,#6307,#6308,#6309,#6310),.UNSPECIFIED.,.F.,.F.,(4,3,3,
3,3,3,3,3,4),(32.7252629519544,32.7784850044617,33.7717724288393,34.7650598532169,
35.7583472775945,36.7516347019722,37.7449221263498,38.7382095507274,39.008448259134),
 .UNSPECIFIED.);
#135=B_SPLINE_CURVE_WITH_KNOTS('',3,(#6311,#6312,#6313,#6314,#6315,#6316,
#6317,#6318,#6319,#6320,#6321,#6322,#6323,#6324,#6325,#6326,#6327,#6328,
#6329,#6330,#6331,#6332),.UNSPECIFIED.,.F.,.F.,(4,3,3,3,3,3,3,4),(-35.2569655693205,
-34.7650598532169,-33.7717724288393,-32.7784850044617,-31.785197580084,
-30.7919101557064,-29.7986227313288,-28.973780262141),.UNSPECIFIED.);
#136=B_SPLINE_CURVE_WITH_KNOTS('',3,(#6337,#6338,#6339,#6340,#6341,#6342,
#6343,#6344,#6345,#6346,#6347,#6348,#6349,#6350,#6351,#6352,#6353,#6354,
#6355,#6356,#6357,#6358),.UNSPECIFIED.,.F.,.F.,(4,3,3,3,3,3,3,4),(26.4420776447749,
26.8187604581959,27.8120478825735,28.8053353069512,29.7986227313288,30.7919101557064,
31.785197580084,32.7252629519544),.UNSPECIFIED.);
#137=B_SPLINE_CURVE_WITH_KNOTS('',3,(#6359,#6360,#6361,#6362,#6363,#6364,
#6365,#6366,#6367,#6368,#6369,#6370,#6371,#6372,#6373,#6374,#6375,#6376,
#6377,#6378,#6379,#6380,#6381,#6382,#6383),.UNSPECIFIED.,.F.,.F.,(4,3,3,
3,3,3,3,3,4),(-28.973780262141,-28.8053353069512,-27.8120478825735,-26.8187604581959,
-25.8254730338183,-24.8321856094406,-23.838898185063,-22.8456107606854,
-22.6905949549614),.UNSPECIFIED.);
#138=B_SPLINE_CURVE_WITH_KNOTS('',3,(#6388,#6389,#6390,#6391,#6392,#6393,
#6394,#6395,#6396,#6397,#6398,#6399,#6400,#6401,#6402,#6403,#6404,#6405,
#6406,#6407,#6408,#6409),.UNSPECIFIED.,.F.,.F.,(4,3,3,3,3,3,3,4),(20.1588923375953,
20.8590359119301,21.8523233363078,22.8456107606854,23.838898185063,24.8321856094406,
25.8254730338183,26.4420776447749),.UNSPECIFIED.);
#139=B_SPLINE_CURVE_WITH_KNOTS('',3,(#6410,#6411,#6412,#6413,#6414,#6415,
#6416,#6417,#6418,#6419,#6420,#6421,#6422,#6423,#6424,#6425,#6426,#6427,
#6428,#6429,#6430,#6431),.UNSPECIFIED.,.F.,.F.,(4,3,3,3,3,3,3,4),(-22.6905949549614,
-21.8523233363078,-20.8590359119301,-19.8657484875525,-18.8724610631749,
-17.8791736387973,-16.8858862144196,-16.4074096477818),.UNSPECIFIED.);
#140=B_SPLINE_CURVE_WITH_KNOTS('',3,(#6436,#6437,#6438,#6439,#6440,#6441,
#6442,#6443,#6444,#6445,#6446,#6447,#6448,#6449,#6450,#6451,#6452,#6453,
#6454,#6455,#6456,#6457,#6458,#6459,#6460),.UNSPECIFIED.,.F.,.F.,(4,3,3,
3,3,3,3,3,4),(13.8757070304157,13.9060239412868,14.8993113656644,15.892598790042,
16.8858862144196,17.8791736387973,18.8724610631749,19.8657484875525,20.1588923375953),
 .UNSPECIFIED.);
#141=B_SPLINE_CURVE_WITH_KNOTS('',3,(#6461,#6462,#6463,#6464,#6465,#6466,
#6467,#6468,#6469,#6470,#6471,#6472,#6473,#6474,#6475,#6476,#6477,#6478,
#6479,#6480,#6481,#6482),.UNSPECIFIED.,.F.,.F.,(4,3,3,3,3,3,3,4),(-16.4074096477818,
-15.892598790042,-14.8993113656644,-13.9060239412868,-12.9127365169091,
-11.9194490925315,-10.9261616681539,-10.1242243406022),.UNSPECIFIED.);
#142=B_SPLINE_CURVE_WITH_KNOTS('',3,(#6488,#6489,#6490,#6491,#6492,#6493,
#6494,#6495,#6496,#6497,#6498,#6499,#6500),.UNSPECIFIED.,.F.,.F.,(4,3,3,
3,4),(-3.84103903342261,-2.97986227313288,-1.98657484875525,-0.993287424377625,
0.),.UNSPECIFIED.);
#143=B_SPLINE_CURVE_WITH_KNOTS('',3,(#6503,#6504,#6505,#6506,#6507,#6508,
#6509,#6510,#6511,#6512,#6513,#6514,#6515,#6516,#6517,#6518,#6519,#6520,
#6521),.UNSPECIFIED.,.F.,.F.,(4,3,3,3,3,3,4),(2.00878279588941,2.97986227313288,
3.9731496975105,4.96643712188813,5.95972454626575,6.95301197064338,7.5925217232361),
 .UNSPECIFIED.);
#144=B_SPLINE_CURVE_WITH_KNOTS('',3,(#6527,#6528,#6529,#6530,#6531,#6532),
 .UNSPECIFIED.,.F.,.F.,(4,1,1,4),(97.3893722612836,98.2829301553797,99.2762175797573,
100.269505004135),.UNSPECIFIED.);
#145=B_SPLINE_CURVE_WITH_KNOTS('',3,(#6535,#6536,#6537,#6538,#6539,#6540,
#6541),.UNSPECIFIED.,.F.,.F.,(4,1,1,1,4),(97.3893722612836,97.8347704996129,
98.8280579239905,99.8213453483681,100.792424825612),.UNSPECIFIED.);
#146=B_SPLINE_CURVE_WITH_KNOTS('',3,(#6546,#6547,#6548,#6549,#6550,#6551,
#6552,#6553,#6554,#6555,#6556),.UNSPECIFIED.,.F.,.F.,(4,1,1,1,1,1,1,1,4),
(91.106186954104,91.3299181847363,92.323205609114,93.3164930334916,94.3097804578692,
95.3030678822468,96.2963553066245,97.2896427310021,97.3893722612836),
 .UNSPECIFIED.);
#147=B_SPLINE_CURVE_WITH_KNOTS('',3,(#6557,#6558,#6559,#6560,#6561,#6562,
#6563,#6564,#6565,#6566),.UNSPECIFIED.,.F.,.F.,(4,1,1,1,1,1,1,4),(91.106186954104,
91.8750459533471,92.8683333777248,93.8616208021024,94.85490822648,95.8481956508576,
96.8414830752353,97.3893722612836),.UNSPECIFIED.);
#148=B_SPLINE_CURVE_WITH_KNOTS('',3,(#6571,#6572,#6573,#6574,#6575,#6576,
#6577,#6578,#6579,#6580),.UNSPECIFIED.,.F.,.F.,(4,1,1,1,1,1,1,4),(84.8230016469244,
85.3701936384706,86.3634810628482,87.3567684872258,88.3500559116035,89.3433433359811,
90.3366307603587,91.106186954104),.UNSPECIFIED.);
#149=B_SPLINE_CURVE_WITH_KNOTS('',3,(#6581,#6582,#6583,#6584,#6585,#6586,
#6587,#6588,#6589,#6590,#6591),.UNSPECIFIED.,.F.,.F.,(4,1,1,1,1,1,1,1,4),
(84.8230016469244,84.9220339827037,85.9153214070814,86.908608831459,87.9018962558366,
88.8951836802142,89.8884711045919,90.8817585289695,91.106186954104),
 .UNSPECIFIED.);
#150=B_SPLINE_CURVE_WITH_KNOTS('',3,(#6596,#6597,#6598,#6599,#6600,#6601,
#6602,#6603,#6604,#6605),.UNSPECIFIED.,.F.,.F.,(4,1,1,1,1,1,1,4),(78.5398163397448,
79.4104690922048,80.4037565165825,81.3970439409601,82.3903313653377,83.3836187897153,
84.376906214093,84.8230016469244),.UNSPECIFIED.);
#151=B_SPLINE_CURVE_WITH_KNOTS('',3,(#6606,#6607,#6608,#6609,#6610,#6611,
#6612,#6613,#6614,#6615),.UNSPECIFIED.,.F.,.F.,(4,1,1,1,1,1,1,4),(78.5398163397448,
78.962309436438,79.9555968608156,80.9488842851932,81.9421717095709,82.9354591339485,
83.9287465583261,84.8230016469244),.UNSPECIFIED.);
#152=B_SPLINE_CURVE_WITH_KNOTS('',3,(#6620,#6621,#6622,#6623,#6624,#6625,
#6626,#6627,#6628,#6629,#6630),.UNSPECIFIED.,.F.,.F.,(4,1,1,1,1,1,1,1,4),
(72.2566310325652,72.4574571215614,73.4507445459391,74.4440319703167,75.4373193946943,
76.430606819072,77.4238942434496,78.4171816678272,78.5398163397448),
 .UNSPECIFIED.);
#153=B_SPLINE_CURVE_WITH_KNOTS('',3,(#6631,#6632,#6633,#6634,#6635,#6636,
#6637,#6638,#6639,#6640),.UNSPECIFIED.,.F.,.F.,(4,1,1,1,1,1,1,4),(72.2566310325652,
73.0025848901722,73.9958723145499,74.9891597389275,75.9824471633051,76.9757345876827,
77.9690220120604,78.5398163397448),.UNSPECIFIED.);
#154=B_SPLINE_CURVE_WITH_KNOTS('',3,(#6645,#6646,#6647,#6648,#6649,#6650,
#6651,#6652,#6653,#6654),.UNSPECIFIED.,.F.,.F.,(4,1,1,1,1,1,1,4),(65.9734457253856,
66.4977325752957,67.4910199996733,68.4843074240509,69.4775948484286,70.4708822728062,
71.4641696971838,72.2566310325652),.UNSPECIFIED.);
#155=B_SPLINE_CURVE_WITH_KNOTS('',3,(#6655,#6656,#6657,#6658,#6659,#6660,
#6661,#6662,#6663,#6664,#6665),.UNSPECIFIED.,.F.,.F.,(4,1,1,1,1,1,1,1,4),
(65.9734457253856,66.0495729195289,67.0428603439065,68.0361477682841,69.0294351926617,
70.0227226170393,71.016010041417,72.0092974657946,72.2566310325652),
 .UNSPECIFIED.);
#156=B_SPLINE_CURVE_WITH_KNOTS('',3,(#6670,#6671,#6672,#6673,#6674,#6675,
#6676,#6677,#6678,#6679),.UNSPECIFIED.,.F.,.F.,(4,1,1,1,1,1,1,4),(59.690260418206,
60.5380080290299,61.5312954534076,62.5245828777852,63.5178703021628,64.5111577265404,
65.5044451509181,65.9734457253856),.UNSPECIFIED.);
#157=B_SPLINE_CURVE_WITH_KNOTS('',3,(#6680,#6681,#6682,#6683,#6684,#6685,
#6686,#6687,#6688,#6689),.UNSPECIFIED.,.F.,.F.,(4,1,1,1,1,1,1,4),(59.690260418206,
60.0898483732631,61.0831357976407,62.0764232220183,63.069710646396,64.0629980707736,
65.0562854951512,65.9734457253856),.UNSPECIFIED.);
#158=B_SPLINE_CURVE_WITH_KNOTS('',3,(#6694,#6695,#6696,#6697,#6698,#6699,
#6700,#6701,#6702,#6703,#6704),.UNSPECIFIED.,.F.,.F.,(4,1,1,1,1,1,1,1,4),
(53.4070751110264,53.5849960583866,54.5782834827642,55.5715709071418,56.5648583315194,
57.5581457558971,58.5514331802747,59.5447206046523,59.690260418206),
 .UNSPECIFIED.);
#159=B_SPLINE_CURVE_WITH_KNOTS('',3,(#6705,#6706,#6707,#6708,#6709,#6710,
#6711,#6712,#6713,#6714),.UNSPECIFIED.,.F.,.F.,(4,1,1,1,1,1,1,4),(53.4070751110264,
54.1301238269973,55.123411251375,56.1166986757526,57.1099861001302,58.1032735245078,
59.0965609488855,59.690260418206),.UNSPECIFIED.);
#160=B_SPLINE_CURVE_WITH_KNOTS('',3,(#6719,#6720,#6721,#6722,#6723,#6724,
#6725,#6726,#6727,#6728),.UNSPECIFIED.,.F.,.F.,(4,1,1,1,1,1,1,4),(47.1238898038468,
47.6252715121208,48.6185589364984,49.6118463608761,50.6051337852537,51.5984212096313,
52.5917086340089,53.4070751110264),.UNSPECIFIED.);
#161=B_SPLINE_CURVE_WITH_KNOTS('',3,(#6729,#6730,#6731,#6732,#6733,#6734,
#6735,#6736,#6737,#6738,#6739),.UNSPECIFIED.,.F.,.F.,(4,1,1,1,1,1,1,1,4),
(47.1238898038468,47.177111856354,48.1703992807316,49.1636867051092,50.1569741294868,
51.1502615538645,52.1435489782421,53.1368364026197,53.4070751110264),
 .UNSPECIFIED.);
#162=B_SPLINE_CURVE_WITH_KNOTS('',3,(#6744,#6745,#6746,#6747,#6748,#6749,
#6750,#6751,#6752,#6753),.UNSPECIFIED.,.F.,.F.,(4,1,1,1,1,1,1,4),(40.8407044966673,
41.6655469658551,42.6588343902327,43.6521218146103,44.6454092389879,45.6386966633656,
46.6319840877432,47.1238898038468),.UNSPECIFIED.);
#163=B_SPLINE_CURVE_WITH_KNOTS('',3,(#6754,#6755,#6756,#6757,#6758,#6759,
#6760,#6761,#6762,#6763),.UNSPECIFIED.,.F.,.F.,(4,1,1,1,1,1,1,4),(40.8407044966672,
41.2173873100882,42.2106747344658,43.2039621588435,44.1972495832211,45.1905370075987,
46.1838244319763,47.1238898038468),.UNSPECIFIED.);
#164=B_SPLINE_CURVE_WITH_KNOTS('',3,(#6768,#6769,#6770,#6771,#6772,#6773,
#6774,#6775,#6776,#6777,#6778),.UNSPECIFIED.,.F.,.F.,(4,1,1,1,1,1,1,1,4),
(34.5575191894876,34.7125349952117,35.7058224195893,36.6991098439669,37.6923972683445,
38.6856846927222,39.6789721170998,40.6722595414774,40.8407044966673),
 .UNSPECIFIED.);
#165=B_SPLINE_CURVE_WITH_KNOTS('',3,(#6779,#6780,#6781,#6782,#6783,#6784,
#6785,#6786,#6787,#6788),.UNSPECIFIED.,.F.,.F.,(4,1,1,1,1,1,1,4),(34.5575191894876,
35.2576627638225,36.2509501882001,37.2442376125777,38.2375250369553,39.230812461333,
40.2240998857106,40.8407044966672),.UNSPECIFIED.);
#166=B_SPLINE_CURVE_WITH_KNOTS('',3,(#6793,#6794,#6795,#6796,#6797,#6798,
#6799,#6800,#6801,#6802),.UNSPECIFIED.,.F.,.F.,(4,1,1,1,1,1,1,4),(28.2743338823081,
28.7528104489459,29.7460978733235,30.7393852977012,31.7326727220788,32.7259601464564,
33.719247570834,34.5575191894876),.UNSPECIFIED.);
#167=B_SPLINE_CURVE_WITH_KNOTS('',3,(#6803,#6804,#6805,#6806,#6807,#6808,
#6809,#6810,#6811,#6812,#6813),.UNSPECIFIED.,.F.,.F.,(4,1,1,1,1,1,1,1,4),
(28.2743338823081,28.3046507931791,29.2979382175567,30.2912256419343,31.284513066312,
32.2778004906896,33.2710879150672,34.2643753394448,34.5575191894876),
 .UNSPECIFIED.);
#168=B_SPLINE_CURVE_WITH_KNOTS('',3,(#6818,#6819,#6820,#6821,#6822,#6823,
#6824,#6825,#6826,#6827),.UNSPECIFIED.,.F.,.F.,(4,1,1,1,1,1,1,4),(21.9911485751285,
22.7930859026802,23.7863733270578,24.7796607514354,25.772948175813,26.7662356001907,
27.7595230245683,28.2743338823081),.UNSPECIFIED.);
#169=B_SPLINE_CURVE_WITH_KNOTS('',3,(#6828,#6829,#6830,#6831,#6832,#6833,
#6834,#6835,#6836,#6837),.UNSPECIFIED.,.F.,.F.,(4,1,1,1,1,1,1,4),(21.9911485751285,
22.3449262469133,23.3382136712909,24.3315010956686,25.3247885200462,26.3180759444238,
27.3113633688014,28.2743338823081),.UNSPECIFIED.);
#170=B_SPLINE_CURVE_WITH_KNOTS('',3,(#6843,#6844,#6845,#6846,#6847),
 .UNSPECIFIED.,.F.,.F.,(4,1,4),(14.3986268518923,15.3919142762699,15.7079632679489),
 .UNSPECIFIED.);
#171=B_SPLINE_CURVE_WITH_KNOTS('',3,(#6850,#6851,#6852,#6853,#6854),
 .UNSPECIFIED.,.F.,.F.,(4,1,4),(13.8757070304157,14.8467865076592,15.7079632679489),
 .UNSPECIFIED.);
#172=B_SPLINE_CURVE_WITH_KNOTS('',3,(#6870,#6871,#6872,#6873,#6874,#6875,
#6876,#6877,#6878,#6879,#6880,#6881,#6882,#6883,#6884,#6885,#6886,#6887,
#6888,#6889,#6890,#6891,#6892,#6893,#6894,#6895,#6896,#6897,#6898,#6899,
#6900,#6901,#6902,#6903,#6904,#6905,#6906,#6907,#6908,#6909,#6910,#6911,
#6912,#6913,#6914,#6915,#6916,#6917,#6918,#6919,#6920,#6921,#6922,#6923,
#6924,#6925,#6926,#6927,#6928,#6929,#6930,#6931,#6932,#6933,#6934,#6935,
#6936,#6937,#6938,#6939,#6940,#6941,#6942,#6943,#6944,#6945,#6946,#6947,
#6948,#6949,#6950,#6951,#6952,#6953,#6954,#6955,#6956,#6957),
 .UNSPECIFIED.,.F.,.F.,(4,3,3,3,3,3,3,3,3,3,3,3,3,3,3,3,3,3,3,3,3,3,3,3,
3,3,3,3,3,4),(-0.474022601254863,-0.451447175941748,-0.428273788597453,
-0.423263601228443,-0.399553812376564,-0.380942280379475,-0.374677880834769,
-0.369385014064713,-0.345072731579855,-0.320408625751709,-0.295981811285532,
-0.286035429877351,-0.281943430084052,-0.25663161347214,-0.250661556399856,
-0.226280185736045,-0.201336866368482,-0.195740838705825,-0.190049717983688,
-0.164715513336959,-0.138863642602314,-0.112826574512041,-0.104606258115944,
-0.0991039006760492,-0.0951662220532652,-0.0685013567711513,-0.0418208873497662,
-0.0157306474362453,-0.00570411484459894,0.),.UNSPECIFIED.);
#173=B_SPLINE_CURVE_WITH_KNOTS('',3,(#6958,#6959,#6960,#6961,#6962,#6963,
#6964,#6965,#6966,#6967,#6968,#6969,#6970,#6971,#6972,#6973,#6974,#6975,
#6976,#6977,#6978,#6979,#6980,#6981,#6982,#6983,#6984,#6985,#6986,#6987,
#6988,#6989,#6990,#6991,#6992,#6993,#6994,#6995,#6996,#6997,#6998,#6999,
#7000,#7001,#7002,#7003,#7004,#7005,#7006,#7007,#7008,#7009,#7010,#7011,
#7012,#7013,#7014,#7015,#7016,#7017,#7018,#7019,#7020,#7021,#7022,#7023,
#7024,#7025,#7026,#7027,#7028,#7029,#7030,#7031,#7032,#7033,#7034,#7035,
#7036,#7037,#7038,#7039,#7040,#7041,#7042,#7043,#7044,#7045,#7046,#7047,
#7048),.UNSPECIFIED.,.F.,.F.,(4,3,3,3,3,3,3,3,3,3,3,3,3,3,3,3,3,3,3,3,3,
3,3,3,3,3,3,3,3,3,4),(-0.472119585381858,-0.44577460207496,-0.418546032433648,
-0.413165251718511,-0.407785600416182,-0.381445798916785,-0.362258329670245,
-0.355369245757151,-0.350800797401284,-0.32505688895012,-0.29982216759042,
-0.275104705363238,-0.267797971074288,-0.262198851065717,-0.258325702856778,
-0.233810691839444,-0.227946044944466,-0.20299171843274,-0.178209571955242,
-0.172135092187495,-0.168338367316375,-0.143931769623782,-0.119575292467824,
-0.0956609071136006,-0.085488047709299,-0.0813672853715775,-0.0579089720113479,
-0.0348587622710651,-0.0125514055137675,-0.00473454661276074,0.),
 .UNSPECIFIED.);
#174=B_SPLINE_CURVE_WITH_KNOTS('',3,(#7050,#7051,#7052,#7053,#7054,#7055,
#7056,#7057,#7058,#7059,#7060),.UNSPECIFIED.,.F.,.F.,(4,1,1,1,1,1,1,1,4),
(15.7079632679489,15.8400739320368,16.8333613564144,17.826648780792,18.8199362051697,
19.8132236295473,20.8065110539249,21.7997984783025,21.9911485751285),
 .UNSPECIFIED.);
#175=B_SPLINE_CURVE_WITH_KNOTS('',3,(#7061,#7062,#7063,#7064,#7065,#7066,
#7067,#7068,#7069,#7070),.UNSPECIFIED.,.F.,.F.,(4,1,1,1,1,1,1,4),(15.7079632679489,
16.3852017006476,17.3784891250252,18.3717765494028,19.3650639737804,20.3583513981581,
21.3516388225357,21.9911485751285),.UNSPECIFIED.);
#176=B_SPLINE_CURVE_WITH_KNOTS('',3,(#7439,#7440,#7441,#7442,#7443,#7444,
#7445,#7446,#7447,#7448,#7449,#7450,#7451,#7452,#7453,#7454,#7455,#7456,
#7457,#7458,#7459,#7460,#7461,#7462,#7463,#7464,#7465,#7466,#7467,#7468,
#7469,#7470,#7471,#7472,#7473,#7474,#7475,#7476,#7477,#7478,#7479,#7480,
#7481,#7482,#7483,#7484,#7485,#7486,#7487,#7488,#7489,#7490,#7491,#7492,
#7493,#7494,#7495,#7496,#7497,#7498,#7499,#7500,#7501,#7502,#7503,#7504,
#7505,#7506,#7507,#7508,#7509,#7510,#7511,#7512,#7513,#7514,#7515,#7516,
#7517,#7518,#7519,#7520,#7521,#7522,#7523,#7524,#7525,#7526,#7527,#7528,
#7529),.UNSPECIFIED.,.F.,.F.,(4,3,3,3,3,3,3,3,3,3,3,3,3,3,3,3,3,3,3,3,3,
3,3,3,3,3,3,3,3,3,4),(0.,0.0222952799330679,0.0452097945174155,0.0673981627831887,
0.0771055738994644,0.0835930447079554,0.0876186285667832,0.111617824771073,
0.135994295972414,0.157674907140211,0.166068223331749,0.170734301358664,
0.174713848522195,0.199787338407663,0.222716740643601,0.247155303462719,
0.256497618171605,0.26074445324338,0.264505632816036,0.289747052399726,
0.315274931436527,0.341051827552776,0.351578296876228,0.358096975465089,
0.385181978970206,0.405495731599044,0.412526368251741,0.41821220868089,
0.444807422955841,0.466436989485556,0.472119585381884),.UNSPECIFIED.);
#177=B_SPLINE_CURVE_WITH_KNOTS('',3,(#7530,#7531,#7532,#7533,#7534,#7535,
#7536,#7537,#7538,#7539,#7540,#7541,#7542,#7543,#7544,#7545,#7546,#7547,
#7548,#7549,#7550,#7551,#7552,#7553,#7554),.UNSPECIFIED.,.F.,.F.,(4,3,3,
3,3,3,3,3,4),(-10.1242243406022,-9.93287424377626,-8.93958681939863,-7.946299395021,
-6.95301197064338,-5.95972454626575,-4.96643712188813,-3.9731496975105,
-3.84103903342261),.UNSPECIFIED.);
#178=B_SPLINE_CURVE_WITH_KNOTS('',3,(#7923,#7924,#7925,#7926,#7927,#7928,
#7929,#7930,#7931,#7932,#7933,#7934,#7935,#7936,#7937,#7938,#7939,#7940,
#7941,#7942,#7943,#7944),.UNSPECIFIED.,.F.,.F.,(4,3,3,3,3,3,3,4),(7.5925217232361,
7.946299395021,8.93958681939863,9.93287424377626,10.9261616681539,11.9194490925315,
12.9127365169091,13.8757070304157),.UNSPECIFIED.);
#179=B_SPLINE_CURVE_WITH_KNOTS('',3,(#7945,#7946,#7947,#7948,#7949,#7950,
#7951,#7952,#7953,#7954,#7955,#7956,#7957,#7958,#7959,#7960,#7961,#7962,
#7963,#7964,#7965,#7966,#7967,#7968,#7969,#7970,#7971,#7972,#7973,#7974,
#7975,#7976,#7977,#7978,#7979,#7980,#7981,#7982,#7983,#7984,#7985,#7986,
#7987,#7988,#7989,#7990,#7991,#7992,#7993,#7994,#7995,#7996,#7997,#7998,
#7999,#8000,#8001,#8002,#8003,#8004,#8005,#8006,#8007,#8008,#8009,#8010,
#8011,#8012,#8013,#8014,#8015,#8016,#8017,#8018,#8019,#8020,#8021,#8022,
#8023,#8024,#8025,#8026,#8027,#8028,#8029,#8030,#8031,#8032,#8033,#8034,
#8035),.UNSPECIFIED.,.F.,.F.,(4,3,3,3,3,3,3,3,3,3,3,3,3,3,3,3,3,3,3,3,3,
3,3,3,3,3,3,3,3,3,4),(0.,0.0259340516234306,0.053368683612658,0.077373986603232,
0.0889343286239471,0.0962033318415016,0.100907449948929,0.126912276034724,
0.152761874310813,0.175924182617423,0.186282013485412,0.191317187370802,
0.195407257095002,0.220409182316126,0.24541110753725,0.270731737634532,
0.279140838448213,0.283746551506711,0.287674236654677,0.312284916819144,
0.336926589907284,0.36117345873944,0.370907512364279,0.37536825313801,0.399043742409906,
0.416600959495802,0.422836588536135,0.427178020979947,0.449946450206982,
0.46927261075349,0.474022601254828),.UNSPECIFIED.);
#180=B_SPLINE_CURVE_WITH_KNOTS('',3,(#8038,#8039,#8040,#8041,#8042,#8043,
#8044,#8045,#8046,#8047,#8048,#8049,#8050,#8051,#8052,#8053,#8054,#8055,
#8056,#8057,#8058,#8059,#8060,#8061,#8062,#8063,#8064,#8065,#8066,#8067,
#8068,#8069,#8070,#8071,#8072,#8073,#8074,#8075,#8076,#8077,#8078,#8079,
#8080,#8081,#8082,#8083,#8084,#8085,#8086,#8087,#8088,#8089,#8090,#8091,
#8092,#8093,#8094,#8095,#8096,#8097,#8098,#8099,#8100,#8101,#8102,#8103,
#8104,#8105,#8106,#8107,#8108,#8109,#8110,#8111,#8112,#8113,#8114,#8115,
#8116,#8117,#8118,#8119,#8120,#8121,#8122,#8123,#8124,#8125),
 .UNSPECIFIED.,.F.,.F.,(4,3,3,3,3,3,3,3,3,3,3,3,3,3,3,3,3,3,3,3,3,3,3,3,
3,3,3,3,3,4),(-0.474022601254861,-0.451447164140717,-0.428273767136123,
-0.423263579545402,-0.399553781970167,-0.380942253773878,-0.374677666863019,
-0.369384940914017,-0.34507264958386,-0.320408545071338,-0.295981736703132,
-0.286035177673738,-0.281943454875479,-0.256631639402781,-0.250661556399858,
-0.226280193777327,-0.201336878994557,-0.195740857792063,-0.190049717577327,
-0.164715519332485,-0.138863651462101,-0.112826583581217,-0.104606275686148,
-0.0991040164814279,-0.0951663280195914,-0.0685014645407558,-0.0418209943289155,
-0.0157307547741264,-0.00570411484459894,0.),.UNSPECIFIED.);
#181=B_SPLINE_CURVE_WITH_KNOTS('',3,(#8126,#8127,#8128,#8129,#8130,#8131,
#8132,#8133,#8134,#8135,#8136,#8137,#8138,#8139,#8140,#8141,#8142,#8143,
#8144,#8145,#8146,#8147,#8148,#8149,#8150,#8151,#8152,#8153,#8154,#8155,
#8156,#8157,#8158,#8159,#8160,#8161,#8162,#8163,#8164,#8165,#8166,#8167,
#8168,#8169,#8170,#8171,#8172,#8173,#8174,#8175,#8176,#8177,#8178,#8179,
#8180,#8181,#8182,#8183,#8184,#8185,#8186,#8187,#8188,#8189,#8190,#8191,
#8192,#8193,#8194,#8195,#8196,#8197,#8198,#8199,#8200,#8201,#8202,#8203,
#8204,#8205,#8206,#8207,#8208,#8209,#8210,#8211,#8212,#8213,#8214,#8215,
#8216),.UNSPECIFIED.,.F.,.F.,(4,3,3,3,3,3,3,3,3,3,3,3,3,3,3,3,3,3,3,3,3,
3,3,3,3,3,3,3,3,3,4),(-0.472119585381859,-0.445774611141889,-0.41854604036721,
-0.413165258086392,-0.407785602596351,-0.381445800212958,-0.362258330804396,
-0.355369248347035,-0.350800798519935,-0.325056888599833,-0.299822162923893,
-0.275104697414975,-0.267797956175982,-0.262198802438247,-0.258325632397721,
-0.233810617962332,-0.227946044944459,-0.202991718039396,-0.178209571611067,
-0.172135088823669,-0.168338364331946,-0.143931766984762,-0.119575288853072,
-0.095660898841475,-0.0854880154494424,-0.081367290874658,-0.057908974539604,
-0.0348587585203453,-0.0125513914292997,-0.00473454661275771,0.),
 .UNSPECIFIED.);
#182=B_SPLINE_CURVE_WITH_KNOTS('',3,(#8218,#8219,#8220,#8221,#8222,#8223,
#8224,#8225,#8226,#8227,#8228),.UNSPECIFIED.,.F.,.F.,(4,1,1,1,1,1,1,1,4),
(15.7079632679489,15.8400739320368,16.8333613564144,17.826648780792,18.8199362051697,
19.8132236295473,20.8065110539249,21.7997984783025,21.9911485751285),
 .UNSPECIFIED.);
#183=B_SPLINE_CURVE_WITH_KNOTS('',3,(#8229,#8230,#8231,#8232,#8233,#8234,
#8235,#8236,#8237,#8238),.UNSPECIFIED.,.F.,.F.,(4,1,1,1,1,1,1,4),(15.7079632679489,
16.3852017006476,17.3784891250252,18.3717765494028,19.3650639737804,20.3583513981581,
21.3516388225357,21.9911485751285),.UNSPECIFIED.);
#184=B_SPLINE_CURVE_WITH_KNOTS('',3,(#8607,#8608,#8609,#8610,#8611,#8612,
#8613,#8614,#8615,#8616,#8617,#8618,#8619,#8620,#8621,#8622,#8623,#8624,
#8625,#8626,#8627,#8628,#8629,#8630,#8631,#8632,#8633,#8634,#8635,#8636,
#8637,#8638,#8639,#8640,#8641,#8642,#8643,#8644,#8645,#8646,#8647,#8648,
#8649,#8650,#8651,#8652,#8653,#8654,#8655,#8656,#8657,#8658,#8659,#8660,
#8661,#8662,#8663,#8664,#8665,#8666,#8667,#8668,#8669,#8670,#8671,#8672,
#8673,#8674,#8675,#8676,#8677,#8678,#8679,#8680,#8681,#8682,#8683,#8684,
#8685,#8686,#8687,#8688,#8689,#8690,#8691,#8692,#8693,#8694,#8695,#8696,
#8697),.UNSPECIFIED.,.F.,.F.,(4,3,3,3,3,3,3,3,3,3,3,3,3,3,3,3,3,3,3,3,3,
3,3,3,3,3,3,3,3,3,4),(0.,0.0222952651137365,0.0452097666204725,0.0673981383733636,
0.0771055510152534,0.08359300396032,0.0876186186491862,0.111617805012605,
0.135994272391414,0.157674889454461,0.166068200672421,0.170733863879555,
0.174713775562166,0.199787267862165,0.222716740643601,0.247155310880047,
0.256497643401853,0.260744554886893,0.264505835070973,0.289747229372796,
0.315275115498424,0.341052012614648,0.351578318626618,0.358096973365246,
0.385181977395323,0.405495730417882,0.412526370937833,0.418212210551543,
0.444807425042136,0.466436989485556,0.472119585381884),.UNSPECIFIED.);
#185=B_SPLINE_CURVE_WITH_KNOTS('',3,(#8698,#8699,#8700,#8701,#8702,#8703,
#8704,#8705,#8706,#8707,#8708,#8709,#8710,#8711,#8712,#8713,#8714,#8715,
#8716,#8717,#8718,#8719,#8720,#8721,#8722),.UNSPECIFIED.,.F.,.F.,(4,3,3,
3,3,3,3,3,4),(-10.1242243406022,-9.93287424377626,-8.93958681939863,-7.946299395021,
-6.95301197064338,-5.95972454626575,-4.96643712188813,-3.9731496975105,
-3.84103903342261),.UNSPECIFIED.);
#186=B_SPLINE_CURVE_WITH_KNOTS('',3,(#9091,#9092,#9093,#9094,#9095,#9096,
#9097,#9098,#9099,#9100,#9101,#9102,#9103,#9104,#9105,#9106,#9107,#9108,
#9109,#9110,#9111,#9112),.UNSPECIFIED.,.F.,.F.,(4,3,3,3,3,3,3,4),(7.5925217232361,
7.946299395021,8.93958681939863,9.93287424377626,10.9261616681539,11.9194490925315,
12.9127365169091,13.8757070304157),.UNSPECIFIED.);
#187=B_SPLINE_CURVE_WITH_KNOTS('',3,(#9113,#9114,#9115,#9116,#9117,#9118,
#9119,#9120,#9121,#9122,#9123,#9124,#9125,#9126,#9127,#9128,#9129,#9130,
#9131,#9132,#9133,#9134,#9135,#9136,#9137,#9138,#9139,#9140,#9141,#9142,
#9143,#9144,#9145,#9146,#9147,#9148,#9149,#9150,#9151,#9152,#9153,#9154,
#9155,#9156,#9157,#9158,#9159,#9160,#9161,#9162,#9163,#9164,#9165,#9166,
#9167,#9168,#9169,#9170,#9171,#9172,#9173,#9174,#9175,#9176,#9177,#9178,
#9179,#9180,#9181,#9182,#9183,#9184,#9185,#9186,#9187,#9188,#9189,#9190,
#9191,#9192,#9193,#9194,#9195,#9196,#9197,#9198,#9199,#9200,#9201,#9202,
#9203),.UNSPECIFIED.,.F.,.F.,(4,3,3,3,3,3,3,3,3,3,3,3,3,3,3,3,3,3,3,3,3,
3,3,3,3,3,3,3,3,3,4),(0.,0.0259340620084641,0.0533686926995623,0.0773739945542733,
0.0889343332539756,0.0962033282984184,0.100907449205028,0.126912275229181,
0.152761870371554,0.175924179662978,0.186282012481782,0.191317190306999,
0.195407257920147,0.220409182728698,0.24541110753725,0.270731737938341,
0.279140836043757,0.28374654253246,0.287674221295602,0.312284901472548,
0.336926574293682,0.36117344014891,0.370907500046057,0.37536825002033,0.399043735515415,
0.416600954324934,0.422836562863072,0.427177984470413,0.449946407582691,
0.46927261075349,0.474022601254827),.UNSPECIFIED.);
#188=B_SPLINE_CURVE_WITH_KNOTS('',3,(#9401,#9402,#9403,#9404,#9405,#9406,
#9407,#9408,#9409,#9410),.UNSPECIFIED.,.F.,.F.,(4,3,3,4),(-4.09157007060747,
-3.98888670333582,-2.99166502750187,-2.06659765062436),.UNSPECIFIED.);
#189=B_SPLINE_CURVE_WITH_KNOTS('',3,(#9413,#9414,#9415,#9416,#9417,#9418,
#9419),.UNSPECIFIED.,.F.,.F.,(4,3,4),(0.,0.997591697879869,1.11662023360685),
 .UNSPECIFIED.);
#190=B_SPLINE_CURVE_WITH_KNOTS('',3,(#9424,#9425,#9426,#9427,#9428,#9429,
#9430,#9431,#9432,#9433,#9434,#9435,#9436,#9437,#9438,#9439,#9440,#9441,
#9442,#9443,#9444,#9445),.UNSPECIFIED.,.F.,.F.,(4,3,3,3,3,3,3,4),(-10.3747553777871,
-9.97221675833955,-8.9749950825056,-7.97777340667164,-6.98055173083769,
-5.98333005500373,-4.98610837916977,-4.09157007060747),.UNSPECIFIED.);
#191=B_SPLINE_CURVE_WITH_KNOTS('',3,(#9446,#9447,#9448,#9449,#9450,#9451,
#9452,#9453,#9454,#9455,#9456,#9457,#9458,#9459,#9460,#9461,#9462,#9463,
#9464,#9465,#9466,#9467),.UNSPECIFIED.,.F.,.F.,(4,3,3,3,3,3,3,4),(1.11662023360685,
1.99518339575976,2.99277509363965,3.99036679151954,4.98795848939943,5.98555018727932,
6.98314188515921,7.39980554078643),.UNSPECIFIED.);
#192=B_SPLINE_CURVE_WITH_KNOTS('',3,(#9472,#9473,#9474,#9475,#9476,#9477,
#9478,#9479,#9480,#9481,#9482,#9483,#9484,#9485,#9486,#9487,#9488,#9489,
#9490,#9491,#9492,#9493),.UNSPECIFIED.,.F.,.F.,(4,3,3,3,3,3,3,4),(-16.6579406849666,
-15.9555468133433,-14.9583251375093,-13.9611034616754,-12.9638817858414,
-11.9666601100075,-10.9694384341735,-10.3747553777871),.UNSPECIFIED.);
#193=B_SPLINE_CURVE_WITH_KNOTS('',3,(#9494,#9495,#9496,#9497,#9498,#9499,
#9500,#9501,#9502,#9503,#9504,#9505,#9506,#9507,#9508,#9509,#9510,#9511,
#9512,#9513,#9514,#9515),.UNSPECIFIED.,.F.,.F.,(4,3,3,3,3,3,3,4),(7.39980554078643,
7.9807335830391,8.97832528091898,9.97591697879886,10.9735086766787,11.9711003745586,
12.9686920724385,13.682990847966),.UNSPECIFIED.);
#194=B_SPLINE_CURVE_WITH_KNOTS('',3,(#9520,#9521,#9522,#9523,#9524,#9525,
#9526,#9527,#9528,#9529,#9530,#9531,#9532,#9533,#9534,#9535,#9536,#9537,
#9538,#9539,#9540,#9541,#9542,#9543,#9544),.UNSPECIFIED.,.F.,.F.,(4,3,3,
3,3,3,3,3,4),(-22.9411259921462,-22.936098544181,-21.938876868347,-20.941655192513,
-19.9444335166791,-18.9472118408451,-17.9499901650112,-16.9527684891772,
-16.6579406849666),.UNSPECIFIED.);
#195=B_SPLINE_CURVE_WITH_KNOTS('',3,(#9545,#9546,#9547,#9548,#9549,#9550,
#9551,#9552,#9553,#9554,#9555,#9556,#9557,#9558,#9559,#9560,#9561,#9562,
#9563,#9564,#9565,#9566,#9567,#9568,#9569),.UNSPECIFIED.,.F.,.F.,(4,3,3,
3,3,3,3,3,4),(13.682990847966,13.9662837703184,14.9638754681983,15.9614671660782,
16.959058863958,17.9566505618379,18.9542422597178,19.9518339575977,19.9661761551456),
 .UNSPECIFIED.);
#196=B_SPLINE_CURVE_WITH_KNOTS('',3,(#9574,#9575,#9576,#9577,#9578,#9579,
#9580,#9581,#9582,#9583,#9584,#9585,#9586,#9587,#9588,#9589,#9590,#9591,
#9592,#9593,#9594,#9595),.UNSPECIFIED.,.F.,.F.,(4,3,3,3,3,3,3,4),(-29.2243112993258,
-28.9194285991847,-27.9222069233507,-26.9249852475168,-25.9277635716828,
-24.9305418958489,-23.9333202200149,-22.9411259921462),.UNSPECIFIED.);
#197=B_SPLINE_CURVE_WITH_KNOTS('',3,(#9596,#9597,#9598,#9599,#9600,#9601,
#9602,#9603,#9604,#9605,#9606,#9607,#9608,#9609,#9610,#9611,#9612,#9613,
#9614,#9615,#9616,#9617),.UNSPECIFIED.,.F.,.F.,(4,3,3,3,3,3,3,4),(19.9661761551456,
20.9494256554776,21.9470173533575,22.9446090512374,23.9422007491172,24.9397924469971,
25.937384144877,26.2493614623252),.UNSPECIFIED.);
#198=B_SPLINE_CURVE_WITH_KNOTS('',3,(#9622,#9623,#9624,#9625,#9626,#9627,
#9628,#9629,#9630,#9631,#9632,#9633,#9634,#9635,#9636,#9637,#9638,#9639,
#9640,#9641,#9642,#9643),.UNSPECIFIED.,.F.,.F.,(4,3,3,3,3,3,3,4),(-35.5074966065054,
-34.9027586541884,-33.9055369783545,-32.9083153025205,-31.9110936266866,
-30.9138719508526,-29.9166502750186,-29.2243112993258),.UNSPECIFIED.);
#199=B_SPLINE_CURVE_WITH_KNOTS('',3,(#9644,#9645,#9646,#9647,#9648,#9649,
#9650,#9651,#9652,#9653,#9654,#9655,#9656,#9657,#9658,#9659,#9660,#9661,
#9662,#9663,#9664,#9665),.UNSPECIFIED.,.F.,.F.,(4,3,3,3,3,3,3,4),(26.2493614623252,
26.9349758427569,27.9325675406368,28.9301592385167,29.9277509363966,30.9253426342764,
31.9229343321563,32.5325467695048),.UNSPECIFIED.);
#200=B_SPLINE_CURVE_WITH_KNOTS('',3,(#9670,#9671,#9672,#9673,#9674,#9675,
#9676,#9677,#9678,#9679,#9680,#9681,#9682,#9683,#9684,#9685,#9686,#9687,
#9688,#9689,#9690,#9691),.UNSPECIFIED.,.F.,.F.,(4,3,3,3,3,3,3,4),(-41.790681913685,
-40.8860887091922,-39.8888670333582,-38.8916453575242,-37.8944236816903,
-36.8972020058563,-35.8999803300224,-35.5074966065054),.UNSPECIFIED.);
#201=B_SPLINE_CURVE_WITH_KNOTS('',3,(#9692,#9693,#9694,#9695,#9696,#9697,
#9698,#9699,#9700,#9701,#9702,#9703,#9704,#9705,#9706,#9707,#9708,#9709,
#9710,#9711,#9712,#9713),.UNSPECIFIED.,.F.,.F.,(4,3,3,3,3,3,3,4),(32.5325467695048,
32.9205260300362,33.9181177279161,34.915709425796,35.9133011236759,36.9108928215558,
37.9084845194357,38.8157320766844),.UNSPECIFIED.);
#202=B_SPLINE_CURVE_WITH_KNOTS('',3,(#9718,#9719,#9720,#9721,#9722,#9723,
#9724,#9725,#9726,#9727,#9728,#9729,#9730,#9731,#9732,#9733,#9734,#9735,
#9736,#9737,#9738,#9739,#9740,#9741,#9742),.UNSPECIFIED.,.F.,.F.,(4,3,3,
3,3,3,3,3,4),(-48.0738672208646,-47.8666404400298,-46.8694187641959,-45.8721970883619,
-44.874975412528,-43.877753736694,-42.8805320608601,-41.8833103850261,-41.790681913685),
 .UNSPECIFIED.);
#203=B_SPLINE_CURVE_WITH_KNOTS('',3,(#9743,#9744,#9745,#9746,#9747,#9748,
#9749,#9750,#9751,#9752,#9753,#9754,#9755,#9756,#9757,#9758,#9759,#9760,
#9761,#9762,#9763,#9764,#9765,#9766,#9767),.UNSPECIFIED.,.F.,.F.,(4,3,3,
3,3,3,3,3,4),(38.8157320766844,38.9060762173155,39.9036679151954,40.9012596130753,
41.8988513109552,42.8964430088351,43.8940347067149,44.8916264045948,45.098917383864),
 .UNSPECIFIED.);
#204=B_SPLINE_CURVE_WITH_KNOTS('',3,(#9772,#9773,#9774,#9775,#9776,#9777,
#9778,#9779,#9780,#9781,#9782,#9783,#9784,#9785,#9786,#9787,#9788,#9789,
#9790,#9791,#9792,#9793),.UNSPECIFIED.,.F.,.F.,(4,3,3,3,3,3,3,4),(-54.3570525280442,
-53.8499704950336,-52.8527488191996,-51.8555271433657,-50.8583054675317,
-49.8610837916978,-48.8638621158638,-48.0738672208646),.UNSPECIFIED.);
#205=B_SPLINE_CURVE_WITH_KNOTS('',3,(#9794,#9795,#9796,#9797,#9798,#9799,
#9800,#9801,#9802,#9803,#9804,#9805,#9806,#9807,#9808,#9809,#9810,#9811,
#9812,#9813,#9814,#9815),.UNSPECIFIED.,.F.,.F.,(4,3,3,3,3,3,3,4),(45.098917383864,
45.8892181024747,46.8868098003546,47.8844014982345,48.8819931961144,49.8795848939942,
50.8771765918741,51.3821026910436),.UNSPECIFIED.);
#206=B_SPLINE_CURVE_WITH_KNOTS('',3,(#9820,#9821,#9822,#9823,#9824,#9825,
#9826,#9827,#9828,#9829,#9830,#9831,#9832,#9833,#9834,#9835,#9836,#9837,
#9838,#9839,#9840,#9841),.UNSPECIFIED.,.F.,.F.,(4,3,3,3,3,3,3,4),(-60.6402378352238,
-59.8333005500373,-58.8360788742033,-57.8388571983694,-56.8416355225354,
-55.8444138467015,-54.8471921708675,-54.3570525280442),.UNSPECIFIED.);
#207=B_SPLINE_CURVE_WITH_KNOTS('',3,(#9842,#9843,#9844,#9845,#9846,#9847,
#9848,#9849,#9850,#9851,#9852,#9853,#9854,#9855,#9856,#9857,#9858,#9859,
#9860,#9861,#9862,#9863),.UNSPECIFIED.,.F.,.F.,(4,3,3,3,3,3,3,4),(51.3821026910436,
51.874768289754,52.8723599876339,53.8699516855138,54.8675433833937,55.8651350812736,
56.8627267791534,57.6652879982231),.UNSPECIFIED.);
#208=B_SPLINE_CURVE_WITH_KNOTS('',3,(#9868,#9869,#9870,#9871,#9872,#9873,
#9874,#9875,#9876,#9877,#9878,#9879,#9880,#9881,#9882,#9883,#9884,#9885,
#9886,#9887,#9888,#9889,#9890,#9891,#9892),.UNSPECIFIED.,.F.,.F.,(4,3,3,
3,3,3,3,3,4),(-66.9234231424034,-66.813852280875,-65.816630605041,-64.8194089292071,
-63.8221872533731,-62.8249655775391,-61.8277439017052,-60.8305222258712,
-60.6402378352238),.UNSPECIFIED.);
#209=B_SPLINE_CURVE_WITH_KNOTS('',3,(#9893,#9894,#9895,#9896,#9897,#9898,
#9899,#9900,#9901,#9902,#9903,#9904,#9905,#9906,#9907,#9908,#9909,#9910,
#9911,#9912,#9913,#9914,#9915,#9916,#9917),.UNSPECIFIED.,.F.,.F.,(4,3,3,
3,3,3,3,3,4),(57.6652879982231,57.8603184770333,58.8579101749132,59.8555018727931,
60.853093570673,61.8506852685529,62.8482769664328,63.8458686643126,63.9484733054027),
 .UNSPECIFIED.);
#210=B_SPLINE_CURVE_WITH_KNOTS('',3,(#9922,#9923,#9924,#9925,#9926,#9927,
#9928,#9929,#9930,#9931,#9932,#9933,#9934,#9935,#9936,#9937,#9938,#9939,
#9940,#9941,#9942,#9943),.UNSPECIFIED.,.F.,.F.,(4,3,3,3,3,3,3,4),(-73.206608449583,
-72.7971823358787,-71.7999606600447,-70.8027389842108,-69.8055173083768,
-68.8082956325429,-67.8110739567089,-66.9234231424034),.UNSPECIFIED.);
#211=B_SPLINE_CURVE_WITH_KNOTS('',3,(#9944,#9945,#9946,#9947,#9948,#9949,
#9950,#9951,#9952,#9953,#9954,#9955,#9956,#9957,#9958,#9959,#9960,#9961,
#9962,#9963,#9964,#9965),.UNSPECIFIED.,.F.,.F.,(4,3,3,3,3,3,3,4),(63.9484733054027,
64.8434603621925,65.8410520600724,66.8386437579523,67.8362354558322,68.8338271537121,
69.8314188515919,70.2316586125823),.UNSPECIFIED.);
#212=B_SPLINE_CURVE_WITH_KNOTS('',3,(#9970,#9971,#9972,#9973,#9974,#9975,
#9976,#9977,#9978,#9979,#9980,#9981,#9982,#9983,#9984,#9985,#9986,#9987,
#9988,#9989,#9990,#9991),.UNSPECIFIED.,.F.,.F.,(4,3,3,3,3,3,3,4),(-79.4897937567626,
-78.7805123908824,-77.7832907150485,-76.7860690392145,-75.7888473633806,
-74.7916256875466,-73.7944040117127,-73.206608449583),.UNSPECIFIED.);
#213=B_SPLINE_CURVE_WITH_KNOTS('',3,(#9992,#9993,#9994,#9995,#9996,#9997,
#9998,#9999,#10000,#10001,#10002,#10003,#10004,#10005,#10006,#10007,#10008,
#10009,#10010,#10011,#10012,#10013),.UNSPECIFIED.,.F.,.F.,(4,3,3,3,3,3,
3,4),(70.2316586125823,70.8290105494718,71.8266022473517,72.8241939452316,
73.8217856431115,74.8193773409914,75.8169690388713,76.5148439197619),
 .UNSPECIFIED.);
#214=B_SPLINE_CURVE_WITH_KNOTS('',3,(#10018,#10019,#10020,#10021,#10022,
#10023,#10024,#10025,#10026,#10027,#10028,#10029,#10030,#10031,#10032,#10033,
#10034,#10035,#10036,#10037,#10038,#10039,#10040,#10041,#10042),
 .UNSPECIFIED.,.F.,.F.,(4,3,3,3,3,3,3,3,4),(-85.7729790639421,-85.7610641217201,
-84.7638424458862,-83.7666207700522,-82.7693990942182,-81.7721774183843,
-80.7749557425504,-79.7777340667164,-79.4897937567626),.UNSPECIFIED.);
#215=B_SPLINE_CURVE_WITH_KNOTS('',3,(#10043,#10044,#10045,#10046,#10047,
#10048,#10049,#10050,#10051,#10052,#10053,#10054,#10055,#10056,#10057,#10058,
#10059,#10060,#10061,#10062,#10063,#10064),.UNSPECIFIED.,.F.,.F.,(4,3,3,
3,3,3,3,4),(76.5148439197619,76.8145607367511,77.812152434631,78.8097441325109,
79.8073358303908,80.8049275282707,81.8025192261506,82.7980292269415),
 .UNSPECIFIED.);
#216=B_SPLINE_CURVE_WITH_KNOTS('',3,(#10069,#10070,#10071,#10072,#10073,
#10074,#10075,#10076,#10077,#10078,#10079,#10080,#10081,#10082,#10083,#10084,
#10085,#10086,#10087,#10088,#10089,#10090),.UNSPECIFIED.,.F.,.F.,(4,3,3,
3,3,3,3,4),(-92.0561643711217,-91.7443941767238,-90.7471725008899,-89.7499508250559,
-88.752729149222,-87.755507473388,-86.7582857975541,-85.7729790639421),
 .UNSPECIFIED.);
#217=B_SPLINE_CURVE_WITH_KNOTS('',3,(#10091,#10092,#10093,#10094,#10095,
#10096,#10097,#10098,#10099,#10100,#10101,#10102,#10103,#10104,#10105,#10106,
#10107,#10108,#10109,#10110,#10111,#10112),.UNSPECIFIED.,.F.,.F.,(4,3,3,
3,3,3,3,4),(82.7980292269415,83.7977026219104,84.7952943197902,85.7928860176701,
86.79047771555,87.7880694134299,88.7856611113098,89.0812145341211),
 .UNSPECIFIED.);
#218=B_SPLINE_CURVE_WITH_KNOTS('',3,(#10117,#10118,#10119,#10120,#10121,
#10122,#10123,#10124,#10125,#10126,#10127,#10128,#10129,#10130,#10131,#10132,
#10133,#10134,#10135,#10136,#10137,#10138),.UNSPECIFIED.,.F.,.F.,(4,3,3,
3,3,3,3,4),(-98.3393496783013,-97.7277242317276,-96.7305025558936,-95.7332808800597,
-94.7360592042257,-93.7388375283918,-92.7416158525578,-92.0561643711217),
 .UNSPECIFIED.);
#219=B_SPLINE_CURVE_WITH_KNOTS('',3,(#10139,#10140,#10141,#10142,#10143,
#10144,#10145,#10146,#10147,#10148,#10149,#10150,#10151,#10152,#10153,#10154,
#10155,#10156,#10157,#10158,#10159,#10160),.UNSPECIFIED.,.F.,.F.,(4,3,3,
3,3,3,3,4),(89.0812145341211,89.7832528091896,90.7808445070695,91.7784362049494,
92.7760279028293,93.7736196007092,94.771211298589,95.3643998413007),
 .UNSPECIFIED.);
#220=B_SPLINE_CURVE_WITH_KNOTS('',3,(#10165,#10166,#10167,#10168,#10169,
#10170,#10171,#10172,#10173,#10174,#10175,#10176,#10177,#10178,#10179,#10180,
#10181,#10182,#10183,#10184,#10185,#10186),.UNSPECIFIED.,.F.,.F.,(4,3,3,
3,3,3,3,4),(-104.622534985481,-103.711054286731,-102.713832610897,-101.716610935063,
-100.719389259229,-99.7221675833955,-98.7249459075615,-98.3393496783013),
 .UNSPECIFIED.);
#221=B_SPLINE_CURVE_WITH_KNOTS('',3,(#10187,#10188,#10189,#10190,#10191,
#10192,#10193,#10194,#10195,#10196,#10197,#10198,#10199,#10200,#10201,#10202,
#10203,#10204,#10205,#10206,#10207,#10208),.UNSPECIFIED.,.F.,.F.,(4,3,3,
3,3,3,3,4),(95.3643998413007,95.7688029964689,96.7663946943488,97.7639863922287,
98.7615780901086,99.7591697879885,100.756761485868,101.64758514848),
 .UNSPECIFIED.);
#222=B_SPLINE_CURVE_WITH_KNOTS('',3,(#10213,#10214,#10215,#10216,#10217,
#10218,#10219,#10220,#10221,#10222,#10223,#10224,#10225,#10226,#10227,#10228,
#10229,#10230,#10231,#10232,#10233,#10234,#10235,#10236,#10237),
 .UNSPECIFIED.,.F.,.F.,(4,3,3,3,3,3,3,3,4),(-110.905720292661,-110.691606017569,
-109.694384341735,-108.697162665901,-107.699940990067,-106.702719314233,
-105.705497638399,-104.708275962565,-104.622534985481),.UNSPECIFIED.);
#223=B_SPLINE_CURVE_WITH_KNOTS('',3,(#10238,#10239,#10240,#10241,#10242,
#10243,#10244,#10245,#10246,#10247,#10248,#10249,#10250,#10251,#10252,#10253,
#10254,#10255,#10256,#10257,#10258,#10259,#10260,#10261,#10262),
 .UNSPECIFIED.,.F.,.F.,(4,3,3,3,3,3,3,3,4),(101.64758514848,101.754353183748,
102.751944881628,103.749536579508,104.747128277388,105.744719975268,106.742311673148,
107.739903371028,107.93077045566),.UNSPECIFIED.);
#224=B_SPLINE_CURVE_WITH_KNOTS('',3,(#10267,#10268,#10269,#10270,#10271,
#10272,#10273,#10274,#10275,#10276,#10277,#10278,#10279,#10280,#10281,#10282,
#10283,#10284,#10285,#10286,#10287,#10288),.UNSPECIFIED.,.F.,.F.,(4,3,3,
3,3,3,3,4),(-117.18890559984,-116.674936072573,-115.677714396739,-114.680492720905,
-113.683271045071,-112.686049369237,-111.688827693403,-110.905720292661),
 .UNSPECIFIED.);
#225=B_SPLINE_CURVE_WITH_KNOTS('',3,(#10289,#10290,#10291,#10292,#10293,
#10294,#10295,#10296,#10297,#10298,#10299,#10300,#10301,#10302,#10303,#10304,
#10305,#10306,#10307,#10308,#10309,#10310),.UNSPECIFIED.,.F.,.F.,(4,3,3,
3,3,3,3,4),(107.93077045566,108.737495068907,109.735086766787,110.732678464667,
111.730270162547,112.727861860427,113.725453558307,114.213955762839),
 .UNSPECIFIED.);
#226=B_SPLINE_CURVE_WITH_KNOTS('',3,(#10315,#10316,#10317,#10318,#10319,
#10320,#10321,#10322,#10323,#10324,#10325,#10326,#10327,#10328,#10329,#10330,
#10331,#10332,#10333,#10334,#10335,#10336),.UNSPECIFIED.,.F.,.F.,(4,3,3,
3,3,3,3,4),(-123.47209090702,-122.658266127576,-121.661044451742,-120.663822775909,
-119.666601100075,-118.669379424241,-117.672157748407,-117.18890559984),
 .UNSPECIFIED.);
#227=B_SPLINE_CURVE_WITH_KNOTS('',3,(#10337,#10338,#10339,#10340,#10341,
#10342,#10343,#10344,#10345,#10346,#10347,#10348,#10349,#10350,#10351,#10352,
#10353,#10354,#10355,#10356,#10357,#10358),.UNSPECIFIED.,.F.,.F.,(4,3,3,
3,3,3,3,4),(114.213955762839,114.723045256187,115.720636954067,116.718228651947,
117.715820349826,118.713412047706,119.711003745586,120.497141070019),
 .UNSPECIFIED.);
#228=B_SPLINE_CURVE_WITH_KNOTS('',3,(#10363,#10364,#10365,#10366,#10367,
#10368,#10369,#10370,#10371,#10372,#10373,#10374,#10375,#10376,#10377,#10378,
#10379,#10380,#10381,#10382,#10383,#10384,#10385,#10386,#10387),
 .UNSPECIFIED.,.F.,.F.,(4,3,3,3,3,3,3,3,4),(-129.755276214199,-129.638817858414,
-128.64159618258,-127.644374506746,-126.647152830912,-125.649931155078,
-124.652709479244,-123.65548780341,-123.47209090702),.UNSPECIFIED.);
#229=B_SPLINE_CURVE_WITH_KNOTS('',3,(#10388,#10389,#10390,#10391,#10392,
#10393,#10394,#10395,#10396,#10397,#10398,#10399,#10400,#10401,#10402,#10403,
#10404,#10405,#10406,#10407,#10408,#10409,#10410,#10411,#10412),
 .UNSPECIFIED.,.F.,.F.,(4,3,3,3,3,3,3,3,4),(120.497141070019,120.708595443466,
121.706187141346,122.703778839226,123.701370537106,124.698962234986,125.696553932865,
126.694145630745,126.780326377199),.UNSPECIFIED.);
#230=B_SPLINE_CURVE_WITH_KNOTS('',3,(#10417,#10418,#10419,#10420,#10421,
#10422,#10423,#10424,#10425,#10426,#10427,#10428,#10429,#10430,#10431,#10432,
#10433,#10434,#10435,#10436,#10437,#10438),.UNSPECIFIED.,.F.,.F.,(4,3,3,
3,3,3,3,4),(-136.038461521379,-135.622147913418,-134.624926237584,-133.62770456175,
-132.630482885916,-131.633261210082,-130.636039534248,-129.755276214199),
 .UNSPECIFIED.);
#231=B_SPLINE_CURVE_WITH_KNOTS('',3,(#10439,#10440,#10441,#10442,#10443,
#10444,#10445,#10446,#10447,#10448,#10449,#10450,#10451,#10452,#10453,#10454,
#10455,#10456,#10457,#10458,#10459,#10460),.UNSPECIFIED.,.F.,.F.,(4,3,3,
3,3,3,3,4),(126.780326377199,127.691737328625,128.689329026505,129.686920724385,
130.684512422265,131.682104120145,132.679695818025,133.063511684378),
 .UNSPECIFIED.);
#232=B_SPLINE_CURVE_WITH_KNOTS('',3,(#10465,#10466,#10467,#10468,#10469,
#10470,#10471,#10472,#10473,#10474,#10475,#10476,#10477,#10478,#10479,#10480,
#10481,#10482,#10483,#10484,#10485,#10486),.UNSPECIFIED.,.F.,.F.,(4,3,3,
3,3,3,3,4),(-142.321646828558,-141.605477968422,-140.608256292588,-139.611034616754,
-138.61381294092,-137.616591265086,-136.619369589252,-136.038461521379),
 .UNSPECIFIED.);
#233=B_SPLINE_CURVE_WITH_KNOTS('',3,(#10487,#10488,#10489,#10490,#10491,
#10492,#10493,#10494,#10495,#10496,#10497,#10498,#10499,#10500,#10501,#10502,
#10503,#10504,#10505,#10506,#10507,#10508),.UNSPECIFIED.,.F.,.F.,(4,3,3,
3,3,3,3,4),(133.063511684378,133.677287515905,134.674879213784,135.672470911664,
136.670062609544,137.667654307424,138.665246005304,139.346696991558),
 .UNSPECIFIED.);
#234=B_SPLINE_CURVE_WITH_KNOTS('',3,(#10513,#10514,#10515,#10516,#10517,
#10518,#10519,#10520,#10521,#10522,#10523,#10524,#10525,#10526,#10527,#10528,
#10529,#10530,#10531,#10532,#10533,#10534,#10535,#10536,#10537),
 .UNSPECIFIED.,.F.,.F.,(4,3,3,3,3,3,3,3,4),(-148.604832135738,-148.586029699259,
-147.588808023425,-146.591586347591,-145.594364671757,-144.597142995923,
-143.599921320089,-142.602699644256,-142.321646828558),.UNSPECIFIED.);
#235=B_SPLINE_CURVE_WITH_KNOTS('',3,(#10538,#10539,#10540,#10541,#10542,
#10543,#10544,#10545,#10546,#10547,#10548,#10549,#10550,#10551,#10552,#10553,
#10554,#10555,#10556,#10557,#10558,#10559),.UNSPECIFIED.,.F.,.F.,(4,3,3,
3,3,3,3,4),(139.346696991558,139.662837703184,140.660429401064,141.658021098944,
142.655612796824,143.653204494703,144.650796192583,145.629882298737),
 .UNSPECIFIED.);
#236=B_SPLINE_CURVE_WITH_KNOTS('',3,(#10564,#10565,#10566,#10567,#10568,
#10569,#10570,#10571,#10572,#10573,#10574,#10575,#10576,#10577,#10578,#10579,
#10580,#10581,#10582,#10583,#10584,#10585),.UNSPECIFIED.,.F.,.F.,(4,3,3,
3,3,3,3,4),(-154.888017442918,-154.569359754263,-153.572138078429,-152.574916402595,
-151.577694726761,-150.580473050927,-149.583251375093,-148.604832135738),
 .UNSPECIFIED.);
#237=B_SPLINE_CURVE_WITH_KNOTS('',3,(#10586,#10587,#10588,#10589,#10590,
#10591,#10592,#10593,#10594,#10595,#10596,#10597,#10598,#10599,#10600,#10601,
#10602,#10603,#10604,#10605,#10606,#10607,#10608,#10609,#10610),
 .UNSPECIFIED.,.F.,.F.,(4,3,3,3,3,3,3,3,4),(145.629882298737,145.648387890463,
146.645979588343,147.643571286223,148.641162984103,149.638754681983,150.636346379863,
151.633938077743,151.913067605917),.UNSPECIFIED.);
#238=B_SPLINE_CURVE_WITH_KNOTS('',3,(#10615,#10616,#10617,#10618,#10619,
#10620,#10621,#10622,#10623,#10624,#10625,#10626,#10627,#10628,#10629,#10630,
#10631,#10632,#10633,#10634,#10635,#10636),.UNSPECIFIED.,.F.,.F.,(4,3,3,
3,3,3,3,4),(-161.171202750097,-160.552689809267,-159.555468133433,-158.558246457599,
-157.561024781765,-156.563803105931,-155.566581430097,-154.888017442918),
 .UNSPECIFIED.);
#239=B_SPLINE_CURVE_WITH_KNOTS('',3,(#10637,#10638,#10639,#10640,#10641,
#10642,#10643,#10644,#10645,#10646,#10647,#10648,#10649,#10650,#10651,#10652,
#10653,#10654,#10655,#10656,#10657,#10658),.UNSPECIFIED.,.F.,.F.,(4,3,3,
3,3,3,3,4),(151.913067605917,152.631529775622,153.629121473502,154.626713171382,
155.624304869262,156.621896567142,157.619488265022,158.196252913097),
 .UNSPECIFIED.);
#240=B_SPLINE_CURVE_WITH_KNOTS('',3,(#10663,#10664,#10665,#10666,#10667,
#10668,#10669,#10670,#10671,#10672,#10673,#10674,#10675,#10676,#10677,#10678,
#10679,#10680,#10681,#10682,#10683,#10684),.UNSPECIFIED.,.F.,.F.,(4,3,3,
3,3,3,3,4),(-167.454388057277,-166.53601986427,-165.538798188436,-164.541576512603,
-163.544354836769,-162.547133160935,-161.549911485101,-161.171202750097),
 .UNSPECIFIED.);
#241=B_SPLINE_CURVE_WITH_KNOTS('',3,(#10685,#10686,#10687,#10688,#10689,
#10690,#10691,#10692,#10693,#10694,#10695,#10696,#10697,#10698,#10699,#10700,
#10701,#10702,#10703,#10704,#10705,#10706),.UNSPECIFIED.,.F.,.F.,(4,3,3,
3,3,3,3,4),(158.196252913097,158.617079962902,159.614671660782,160.612263358661,
161.609855056541,162.607446754421,163.605038452301,164.479438220276),
 .UNSPECIFIED.);
#242=B_SPLINE_CURVE_WITH_KNOTS('',3,(#10711,#10712,#10713,#10714,#10715,
#10716,#10717,#10718,#10719,#10720,#10721,#10722,#10723,#10724,#10725,#10726,
#10727,#10728,#10729,#10730,#10731,#10732,#10733,#10734,#10735),
 .UNSPECIFIED.,.F.,.F.,(4,3,3,3,3,3,3,3,4),(-173.737573364456,-173.516571595108,
-172.519349919274,-171.52212824344,-170.524906567606,-169.527684891772,
-168.530463215938,-167.533241540104,-167.454388057277),.UNSPECIFIED.);
#243=B_SPLINE_CURVE_WITH_KNOTS('',3,(#10736,#10737,#10738,#10739,#10740,
#10741,#10742,#10743,#10744,#10745,#10746,#10747,#10748,#10749,#10750,#10751,
#10752,#10753,#10754,#10755,#10756,#10757,#10758,#10759,#10760),
 .UNSPECIFIED.,.F.,.F.,(4,3,3,3,3,3,3,3,4),(164.479438220276,164.602630150181,
165.600221848061,166.597813545941,167.595405243821,168.592996941701,169.59058863958,
170.58818033746,170.762623527456),.UNSPECIFIED.);
#244=B_SPLINE_CURVE_WITH_KNOTS('',3,(#10765,#10766,#10767,#10768,#10769,
#10770,#10771,#10772,#10773,#10774,#10775,#10776,#10777,#10778,#10779,#10780,
#10781,#10782,#10783,#10784,#10785,#10786),.UNSPECIFIED.,.F.,.F.,(4,3,3,
3,3,3,3,4),(-180.020758671636,-179.499901650112,-178.502679974278,-177.505458298444,
-176.50823662261,-175.511014946776,-174.513793270942,-173.737573364456),
 .UNSPECIFIED.);
#245=B_SPLINE_CURVE_WITH_KNOTS('',3,(#10787,#10788,#10789,#10790,#10791,
#10792,#10793,#10794,#10795,#10796,#10797,#10798,#10799,#10800,#10801,#10802,
#10803,#10804,#10805,#10806,#10807,#10808),.UNSPECIFIED.,.F.,.F.,(4,3,3,
3,3,3,3,4),(170.762623527456,171.58577203534,172.58336373322,173.5809554311,
174.57854712898,175.57613882686,176.57373052474,177.045808834635),
 .UNSPECIFIED.);
#246=B_SPLINE_CURVE_WITH_KNOTS('',3,(#10813,#10814,#10815,#10816,#10817,
#10818,#10819,#10820,#10821,#10822,#10823,#10824,#10825,#10826,#10827,#10828,
#10829,#10830,#10831,#10832,#10833,#10834),.UNSPECIFIED.,.F.,.F.,(4,3,3,
3,3,3,3,4),(-186.303943978815,-185.483231705116,-184.486010029282,-183.488788353448,
-182.491566677614,-181.49434500178,-180.497123325946,-180.020758671636),
 .UNSPECIFIED.);
#247=B_SPLINE_CURVE_WITH_KNOTS('',3,(#10835,#10836,#10837,#10838,#10839,
#10840,#10841,#10842,#10843,#10844,#10845,#10846,#10847,#10848,#10849,#10850,
#10851,#10852,#10853,#10854,#10855,#10856),.UNSPECIFIED.,.F.,.F.,(4,3,3,
3,3,3,3,4),(177.045808834635,177.57132222262,178.568913920499,179.566505618379,
180.564097316259,181.561689014139,182.559280712019,183.328994141815),
 .UNSPECIFIED.);
#248=B_SPLINE_CURVE_WITH_KNOTS('',3,(#10862,#10863,#10864,#10865,#10866,
#10867,#10868,#10869,#10870,#10871),.UNSPECIFIED.,.F.,.F.,(4,1,1,1,1,1,
1,4),(197.920337176157,198.096846578291,199.094068254125,200.091289929959,
201.088511605793,202.085733281627,203.082954957461,204.080176633295),
 .UNSPECIFIED.);
#249=B_SPLINE_CURVE_WITH_KNOTS('',3,(#10874,#10875,#10876,#10877,#10878,
#10879,#10880,#10881),.UNSPECIFIED.,.F.,.F.,(4,1,1,1,1,4),(197.920337176157,
198.848172022221,199.845763720101,200.843355417981,201.84094711586,202.83853881374),
 .UNSPECIFIED.);
#250=B_SPLINE_CURVE_WITH_KNOTS('',3,(#10886,#10887,#10888,#10889,#10890,
#10891,#10892,#10893,#10894,#10895),.UNSPECIFIED.,.F.,.F.,(4,1,1,1,1,1,
1,4),(191.637151868977,192.113516523288,193.110738199121,194.107959874955,
195.105181550789,196.102403226623,197.099624902457,197.920337176157),
 .UNSPECIFIED.);
#251=B_SPLINE_CURVE_WITH_KNOTS('',3,(#10896,#10897,#10898,#10899,#10900,
#10901,#10902,#10903,#10904,#10905,#10906),.UNSPECIFIED.,.F.,.F.,(4,1,1,
1,1,1,1,1,4),(191.637151868977,191.865030137062,192.862621834942,193.860213532821,
194.857805230701,195.855396928581,196.852988626461,197.850580324341,197.920337176157),
 .UNSPECIFIED.);
#252=B_SPLINE_CURVE_WITH_KNOTS('',3,(#10911,#10912,#10913,#10914,#10915,
#10916,#10917,#10918,#10919,#10920),.UNSPECIFIED.,.F.,.F.,(4,1,1,1,1,1,
1,4),(185.353966561798,186.130186468284,187.127408144118,188.124629819952,
189.121851495786,190.11907317162,191.116294847454,191.637151868977),
 .UNSPECIFIED.);
#253=B_SPLINE_CURVE_WITH_KNOTS('',3,(#10921,#10922,#10923,#10924,#10925,
#10926,#10927,#10928,#10929,#10930),.UNSPECIFIED.,.F.,.F.,(4,1,1,1,1,1,
1,4),(185.353966561798,185.879479949782,186.877071647662,187.874663345542,
188.872255043422,189.869846741302,190.867438439182,191.637151868977),
 .UNSPECIFIED.);
#254=B_SPLINE_CURVE_WITH_KNOTS('',3,(#10935,#10936,#10937,#10938,#10939,
#10940,#10941,#10942,#10943,#10944,#10945),.UNSPECIFIED.,.F.,.F.,(4,1,1,
1,1,1,1,1,4),(179.070781254618,179.149634737446,180.14685641328,181.144078089114,
182.141299764948,183.138521440782,184.135743116616,185.13296479245,185.353966561798),
 .UNSPECIFIED.);
#255=B_SPLINE_CURVE_WITH_KNOTS('',3,(#10946,#10947,#10948,#10949,#10950,
#10951,#10952,#10953,#10954,#10955),.UNSPECIFIED.,.F.,.F.,(4,1,1,1,1,1,
1,4),(179.070781254618,179.893929762503,180.891521460383,181.889113158263,
182.886704856143,183.884296554023,184.881888251902,185.353966561798),
 .UNSPECIFIED.);
#256=B_SPLINE_CURVE_WITH_KNOTS('',3,(#10960,#10961,#10962,#10963,#10964,
#10965,#10966,#10967,#10968,#10969),.UNSPECIFIED.,.F.,.F.,(4,1,1,1,1,1,
1,4),(172.787595947439,173.166304682442,174.163526358276,175.16074803411,
176.157969709944,177.155191385778,178.152413061612,179.070781254618),
 .UNSPECIFIED.);
#257=B_SPLINE_CURVE_WITH_KNOTS('',3,(#10970,#10971,#10972,#10973,#10974,
#10975,#10976,#10977,#10978,#10979,#10980),.UNSPECIFIED.,.F.,.F.,(4,1,1,
1,1,1,1,1,4),(172.787595947439,172.910787877344,173.908379575224,174.905971273104,
175.903562970983,176.901154668863,177.898746366743,178.896338064623,179.070781254618),
 .UNSPECIFIED.);
#258=B_SPLINE_CURVE_WITH_KNOTS('',3,(#10985,#10986,#10987,#10988,#10989,
#10990,#10991,#10992,#10993,#10994),.UNSPECIFIED.,.F.,.F.,(4,1,1,1,1,1,
1,4),(166.504410640259,167.182974627439,168.180196303273,169.177417979107,
170.17463965494,171.171861330774,172.169083006608,172.787595947439),
 .UNSPECIFIED.);
#259=B_SPLINE_CURVE_WITH_KNOTS('',3,(#10995,#10996,#10997,#10998,#10999,
#11000,#11001,#11002,#11003,#11004),.UNSPECIFIED.,.F.,.F.,(4,1,1,1,1,1,
1,4),(166.504410640259,166.925237690065,167.922829387944,168.920421085824,
169.918012783704,170.915604481584,171.913196179464,172.787595947439),
 .UNSPECIFIED.);
#260=B_SPLINE_CURVE_WITH_KNOTS('',3,(#11009,#11010,#11011,#11012,#11013,
#11014,#11015,#11016,#11017,#11018),.UNSPECIFIED.,.F.,.F.,(4,1,1,1,1,1,
1,4),(160.22122533308,161.199644572435,162.196866248269,163.194087924103,
164.191309599937,165.188531275771,166.185752951605,166.504410640259),
 .UNSPECIFIED.);
#261=B_SPLINE_CURVE_WITH_KNOTS('',3,(#11019,#11020,#11021,#11022,#11023,
#11024,#11025,#11026,#11027,#11028),.UNSPECIFIED.,.F.,.F.,(4,1,1,1,1,1,
1,4),(160.22122533308,160.939687502785,161.937279200665,162.934870898545,
163.932462596425,164.930054294305,165.927645992185,166.504410640259),
 .UNSPECIFIED.);
#262=B_SPLINE_CURVE_WITH_KNOTS('',3,(#11033,#11034,#11035,#11036,#11037,
#11038,#11039,#11040,#11041,#11042,#11043),.UNSPECIFIED.,.F.,.F.,(4,1,1,
1,1,1,1,1,4),(153.9380400259,154.219092841597,155.216314517431,156.213536193265,
157.210757869099,158.207979544933,159.205201220767,160.202422896601,160.22122533308),
 .UNSPECIFIED.);
#263=B_SPLINE_CURVE_WITH_KNOTS('',3,(#11044,#11045,#11046,#11047,#11048,
#11049,#11050,#11051,#11052,#11053,#11054),.UNSPECIFIED.,.F.,.F.,(4,1,1,
1,1,1,1,1,4),(153.9380400259,153.956545617626,154.954137315506,155.951729013386,
156.949320711266,157.946912409146,158.944504107025,159.942095804905,160.22122533308),
 .UNSPECIFIED.);
#264=B_SPLINE_CURVE_WITH_KNOTS('',3,(#11059,#11060,#11061,#11062,#11063,
#11064,#11065,#11066,#11067,#11068),.UNSPECIFIED.,.F.,.F.,(4,1,1,1,1,1,
1,4),(147.65485471872,148.235762786593,149.232984462427,150.230206138261,
151.227427814095,152.224649489929,153.221871165763,153.9380400259),
 .UNSPECIFIED.);
#265=B_SPLINE_CURVE_WITH_KNOTS('',3,(#11069,#11070,#11071,#11072,#11073,
#11074,#11075,#11076,#11077,#11078),.UNSPECIFIED.,.F.,.F.,(4,1,1,1,1,1,
1,4),(147.65485471872,147.970995430347,148.968587128227,149.966178826106,
150.963770523986,151.961362221866,152.958953919746,153.9380400259),
 .UNSPECIFIED.);
#266=B_SPLINE_CURVE_WITH_KNOTS('',3,(#11083,#11084,#11085,#11086,#11087,
#11088,#11089,#11090,#11091,#11092),.UNSPECIFIED.,.F.,.F.,(4,1,1,1,1,1,
1,4),(141.371669411541,142.25243273159,143.249654407424,144.246876083258,
145.244097759092,146.241319434926,147.23854111076,147.65485471872),
 .UNSPECIFIED.);
#267=B_SPLINE_CURVE_WITH_KNOTS('',3,(#11093,#11094,#11095,#11096,#11097,
#11098,#11099,#11100,#11101,#11102),.UNSPECIFIED.,.F.,.F.,(4,1,1,1,1,1,
1,4),(141.371669411541,141.985445243067,142.983036940947,143.980628638827,
144.978220336707,145.975812034587,146.973403732467,147.65485471872),
 .UNSPECIFIED.);
#268=B_SPLINE_CURVE_WITH_KNOTS('',3,(#11107,#11108,#11109,#11110,#11111,
#11112,#11113,#11114,#11115,#11116,#11117),.UNSPECIFIED.,.F.,.F.,(4,1,1,
1,1,1,1,1,4),(135.088484104361,135.271881000752,136.269102676586,137.26632435242,
138.263546028254,139.260767704088,140.257989379922,141.255211055756,141.371669411541),
 .UNSPECIFIED.);
#269=B_SPLINE_CURVE_WITH_KNOTS('',3,(#11118,#11119,#11120,#11121,#11122,
#11123,#11124,#11125,#11126,#11127),.UNSPECIFIED.,.F.,.F.,(4,1,1,1,1,1,
1,4),(135.088484104361,135.999895055788,136.997486753668,137.995078451548,
138.992670149428,139.990261847308,140.987853545188,141.371669411541),
 .UNSPECIFIED.);
#270=B_SPLINE_CURVE_WITH_KNOTS('',3,(#11132,#11133,#11134,#11135,#11136,
#11137,#11138,#11139,#11140,#11141),.UNSPECIFIED.,.F.,.F.,(4,1,1,1,1,1,
1,4),(128.805298797182,129.288550945748,130.285772621582,131.282994297416,
132.28021597325,133.277437649084,134.274659324918,135.088484104361),
 .UNSPECIFIED.);
#271=B_SPLINE_CURVE_WITH_KNOTS('',3,(#11142,#11143,#11144,#11145,#11146,
#11147,#11148,#11149,#11150,#11151,#11152),.UNSPECIFIED.,.F.,.F.,(4,1,1,
1,1,1,1,1,4),(128.805298797182,129.016753170629,130.014344868509,131.011936566389,
132.009528264269,133.007119962148,134.004711660028,135.002303357908,135.088484104361),
 .UNSPECIFIED.);
#272=B_SPLINE_CURVE_WITH_KNOTS('',3,(#11157,#11158,#11159,#11160,#11161,
#11162,#11163,#11164,#11165,#11166),.UNSPECIFIED.,.F.,.F.,(4,1,1,1,1,1,
1,4),(122.522113490002,123.305220890745,124.302442566579,125.299664242413,
126.296885918246,127.29410759408,128.291329269914,128.805298797182),
 .UNSPECIFIED.);
#273=B_SPLINE_CURVE_WITH_KNOTS('',3,(#11167,#11168,#11169,#11170,#11171,
#11172,#11173,#11174,#11175,#11176),.UNSPECIFIED.,.F.,.F.,(4,1,1,1,1,1,
1,4),(122.522113490002,123.03120298335,124.028794681229,125.026386379109,
126.023978076989,127.021569774869,128.019161472749,128.805298797182),
 .UNSPECIFIED.);
#274=B_SPLINE_CURVE_WITH_KNOTS('',3,(#11181,#11182,#11183,#11184,#11185,
#11186,#11187,#11188,#11189,#11190,#11191),.UNSPECIFIED.,.F.,.F.,(4,1,1,
1,1,1,1,1,4),(116.238928182823,116.324669159907,117.321890835741,118.319112511575,
119.316334187409,120.313555863243,121.310777539077,122.307999214911,122.522113490002),
 .UNSPECIFIED.);
#275=B_SPLINE_CURVE_WITH_KNOTS('',3,(#11192,#11193,#11194,#11195,#11196,
#11197,#11198,#11199,#11200,#11201),.UNSPECIFIED.,.F.,.F.,(4,1,1,1,1,1,
1,4),(116.238928182823,117.04565279607,118.04324449395,119.04083619183,
120.03842788971,121.03601958759,122.03361128547,122.522113490002),
 .UNSPECIFIED.);
#276=B_SPLINE_CURVE_WITH_KNOTS('',3,(#11206,#11207,#11208,#11209,#11210,
#11211,#11212,#11213,#11214,#11215),.UNSPECIFIED.,.F.,.F.,(4,1,1,1,1,1,
1,4),(109.955742875643,110.341339104903,111.338560780737,112.335782456571,
113.333004132405,114.330225808239,115.327447484073,116.238928182823),
 .UNSPECIFIED.);
#277=B_SPLINE_CURVE_WITH_KNOTS('',3,(#11216,#11217,#11218,#11219,#11220,
#11221,#11222,#11223,#11224,#11225,#11226),.UNSPECIFIED.,.F.,.F.,(4,1,1,
1,1,1,1,1,4),(109.955742875643,110.062510910911,111.060102608791,112.057694306671,
113.055286004551,114.052877702431,115.050469400311,116.04806109819,116.238928182823),
 .UNSPECIFIED.);
#278=B_SPLINE_CURVE_WITH_KNOTS('',3,(#11231,#11232,#11233,#11234,#11235,
#11236,#11237,#11238,#11239,#11240),.UNSPECIFIED.,.F.,.F.,(4,1,1,1,1,1,
1,4),(103.672557568463,104.358009049899,105.355230725733,106.352452401567,
107.349674077401,108.346895753235,109.344117429069,109.955742875643),
 .UNSPECIFIED.);
#279=B_SPLINE_CURVE_WITH_KNOTS('',3,(#11241,#11242,#11243,#11244,#11245,
#11246,#11247,#11248,#11249,#11250),.UNSPECIFIED.,.F.,.F.,(4,1,1,1,1,1,
1,4),(103.672557568463,104.076960723632,105.074552421512,106.072144119392,
107.069735817271,108.067327515151,109.064919213031,109.955742875643),
 .UNSPECIFIED.);
#280=B_SPLINE_CURVE_WITH_KNOTS('',3,(#11255,#11256,#11257,#11258,#11259,
#11260,#11261,#11262,#11263,#11264),.UNSPECIFIED.,.F.,.F.,(4,1,1,1,1,1,
1,4),(97.3893722612838,98.3746789948957,99.3719006707297,100.369122346564,
101.366344022398,102.363565698232,103.360787374066,103.672557568463),
 .UNSPECIFIED.);
#281=B_SPLINE_CURVE_WITH_KNOTS('',3,(#11265,#11266,#11267,#11268,#11269,
#11270,#11271,#11272,#11273,#11274),.UNSPECIFIED.,.F.,.F.,(4,1,1,1,1,1,
1,4),(97.3893722612838,98.0914105363525,99.0890022342324,100.086593932112,
101.084185629992,102.081777327872,103.079369025752,103.672557568463),
 .UNSPECIFIED.);
#282=B_SPLINE_CURVE_WITH_KNOTS('',3,(#11279,#11280,#11281,#11282,#11283,
#11284,#11285,#11286,#11287,#11288,#11289),.UNSPECIFIED.,.F.,.F.,(4,1,1,
1,1,1,1,1,4),(91.1061869541042,91.3941272640581,92.391348939892,93.388570615726,
94.3857922915599,95.3830139673939,96.3802356432278,97.3774573190618,97.3893722612838),
 .UNSPECIFIED.);
#283=B_SPLINE_CURVE_WITH_KNOTS('',3,(#11290,#11291,#11292,#11293,#11294,
#11295,#11296,#11297,#11298,#11299,#11300),.UNSPECIFIED.,.F.,.F.,(4,1,1,
1,1,1,1,1,4),(91.1061869541042,91.1082686511933,92.1058603490732,93.103452046953,
94.1010437448329,95.0986354427128,96.0962271405927,97.0938188384726,97.3893722612838),
 .UNSPECIFIED.);
#284=B_SPLINE_CURVE_WITH_KNOTS('',3,(#11305,#11306,#11307,#11308,#11309,
#11310,#11311,#11312,#11313,#11314),.UNSPECIFIED.,.F.,.F.,(4,1,1,1,1,1,
1,4),(84.8230016469246,85.4107972090543,86.4080188848883,87.4052405607222,
88.4024622365562,89.3996839123901,90.3969055882241,91.1061869541042),
 .UNSPECIFIED.);
#285=B_SPLINE_CURVE_WITH_KNOTS('',3,(#11315,#11316,#11317,#11318,#11319,
#11320,#11321,#11322,#11323,#11324),.UNSPECIFIED.,.F.,.F.,(4,1,1,1,1,1,
1,4),(84.8230016469246,85.122718463914,86.1203101617938,87.1179018596737,
88.1154935575536,89.1130852554335,90.1106769533134,91.1061869541042),
 .UNSPECIFIED.);
#286=B_SPLINE_CURVE_WITH_KNOTS('',3,(#11329,#11330,#11331,#11332,#11333,
#11334,#11335,#11336,#11337,#11338),.UNSPECIFIED.,.F.,.F.,(4,1,1,1,1,1,
1,4),(78.539816339745,79.4274671540506,80.4246888298845,81.4219105057185,
82.4191321815525,83.4163538573864,84.4135755332204,84.8230016469246),
 .UNSPECIFIED.);
#287=B_SPLINE_CURVE_WITH_KNOTS('',3,(#11339,#11340,#11341,#11342,#11343,
#11344,#11345,#11346,#11347,#11348),.UNSPECIFIED.,.F.,.F.,(4,1,1,1,1,1,
1,4),(78.539816339745,79.1371682766347,80.1347599745145,81.1323516723944,
82.1299433702743,83.1275350681542,84.1251267660341,84.8230016469246),
 .UNSPECIFIED.);
#288=B_SPLINE_CURVE_WITH_KNOTS('',3,(#11353,#11354,#11355,#11356,#11357,
#11358,#11359,#11360,#11361,#11362,#11363),.UNSPECIFIED.,.F.,.F.,(4,1,1,
1,1,1,1,1,4),(72.2566310325654,72.4469154232129,73.4441370990469,74.4413587748808,
75.4385804507148,76.4358021265487,77.4330238023827,78.4302454782166,78.539816339745),
 .UNSPECIFIED.);
#289=B_SPLINE_CURVE_WITH_KNOTS('',3,(#11364,#11365,#11366,#11367,#11368,
#11369,#11370,#11371,#11372,#11373),.UNSPECIFIED.,.F.,.F.,(4,1,1,1,1,1,
1,4),(72.2566310325654,73.1516180893553,74.1492097872352,75.1468014851151,
76.144393182995,77.1419848808749,78.1395765787548,78.539816339745),
 .UNSPECIFIED.);
#290=B_SPLINE_CURVE_WITH_KNOTS('',3,(#11378,#11379,#11380,#11381,#11382,
#11383,#11384,#11385,#11386,#11387),.UNSPECIFIED.,.F.,.F.,(4,1,1,1,1,1,
1,4),(65.9734457253858,66.4635853682092,67.4608070440431,68.4580287198771,
69.455250395711,70.452472071545,71.4496937473789,72.2566310325654),
 .UNSPECIFIED.);
#291=B_SPLINE_CURVE_WITH_KNOTS('',3,(#11388,#11389,#11390,#11391,#11392,
#11393,#11394,#11395,#11396,#11397,#11398),.UNSPECIFIED.,.F.,.F.,(4,1,1,
1,1,1,1,1,4),(65.9734457253858,66.1684762041961,67.166067902076,68.1636595999559,
69.1612512978358,70.1588429957157,71.1564346935956,72.1540263914755,72.2566310325654),
 .UNSPECIFIED.);
#292=B_SPLINE_CURVE_WITH_KNOTS('',3,(#11403,#11404,#11405,#11406,#11407,
#11408,#11409,#11410,#11411,#11412),.UNSPECIFIED.,.F.,.F.,(4,1,1,1,1,1,
1,4),(59.6902604182062,60.4802553132055,61.4774769890394,62.4746986648734,
63.4719203407073,64.4691420165413,65.4663636923752,65.9734457253858),
 .UNSPECIFIED.);
#293=B_SPLINE_CURVE_WITH_KNOTS('',3,(#11413,#11414,#11415,#11416,#11417,
#11418,#11419,#11420,#11421,#11422),.UNSPECIFIED.,.F.,.F.,(4,1,1,1,1,1,
1,4),(59.6902604182062,60.1829260169168,61.1805177147967,62.1781094126766,
63.1757011105565,64.1732928084364,65.1708845063163,65.9734457253858),
 .UNSPECIFIED.);
#294=B_SPLINE_CURVE_WITH_KNOTS('',3,(#11427,#11428,#11429,#11430,#11431,
#11432,#11433,#11434,#11435,#11436,#11437),.UNSPECIFIED.,.F.,.F.,(4,1,1,
1,1,1,1,1,4),(53.4070751110266,53.4997035823678,54.4969252582017,55.4941469340357,
56.4913686098696,57.4885902857036,58.4858119615375,59.4830336373715,59.6902604182062),
 .UNSPECIFIED.);
#295=B_SPLINE_CURVE_WITH_KNOTS('',3,(#11438,#11439,#11440,#11441,#11442,
#11443,#11444,#11445,#11446,#11447),.UNSPECIFIED.,.F.,.F.,(4,1,1,1,1,1,
1,4),(53.4070751110266,54.1973758296375,55.1949675275174,56.1925592253973,
57.1901509232772,58.1877426211571,59.1853343190369,59.6902604182062),
 .UNSPECIFIED.);
#296=B_SPLINE_CURVE_WITH_KNOTS('',3,(#11452,#11453,#11454,#11455,#11456,
#11457,#11458,#11459,#11460,#11461),.UNSPECIFIED.,.F.,.F.,(4,1,1,1,1,1,
1,4),(47.123889803847,47.516373527364,48.513595203198,49.5108168790319,
50.5080385548659,51.5052602306999,52.5024819065338,53.4070751110266),
 .UNSPECIFIED.);
#297=B_SPLINE_CURVE_WITH_KNOTS('',3,(#11462,#11463,#11464,#11465,#11466,
#11467,#11468,#11469,#11470,#11471,#11472),.UNSPECIFIED.,.F.,.F.,(4,1,1,
1,1,1,1,1,4),(47.123889803847,47.2142339444783,48.2118256423582,49.2094173402381,
50.207009038118,51.2046007359979,52.2021924338777,53.1997841317576,53.4070751110266),
 .UNSPECIFIED.);
#298=B_SPLINE_CURVE_WITH_KNOTS('',3,(#11477,#11478,#11479,#11480,#11481,
#11482,#11483,#11484,#11485,#11486),.UNSPECIFIED.,.F.,.F.,(4,1,1,1,1,1,
1,4),(40.8407044966674,41.5330434723603,42.5302651481943,43.5274868240282,
44.5247084998622,45.5219301756961,46.5191518515301,47.123889803847),
 .UNSPECIFIED.);
#299=B_SPLINE_CURVE_WITH_KNOTS('',3,(#11487,#11488,#11489,#11490,#11491,
#11492,#11493,#11494,#11495,#11496),.UNSPECIFIED.,.F.,.F.,(4,1,1,1,1,1,
1,4),(40.8407044966675,41.228683757199,42.2262754550789,43.2238671529588,
44.2214588508387,45.2190505487186,46.2166422465984,47.123889803847),
 .UNSPECIFIED.);
#300=B_SPLINE_CURVE_WITH_KNOTS('',3,(#11501,#11502,#11503,#11504,#11505,
#11506,#11507,#11508,#11509,#11510),.UNSPECIFIED.,.F.,.F.,(4,1,1,1,1,1,
1,4),(34.5575191894878,35.5497134173566,36.5469350931905,37.5441567690245,
38.5413784448584,39.5386001206924,40.5358217965264,40.8407044966674),
 .UNSPECIFIED.);
#301=B_SPLINE_CURVE_WITH_KNOTS('',3,(#11511,#11512,#11513,#11514,#11515,
#11516,#11517,#11518,#11519,#11520),.UNSPECIFIED.,.F.,.F.,(4,1,1,1,1,1,
1,4),(34.5575191894879,35.2431335699197,36.2407252677996,37.2383169656795,
38.2359086635594,39.2335003614392,40.2310920593191,40.8407044966675),
 .UNSPECIFIED.);
#302=B_SPLINE_CURVE_WITH_KNOTS('',3,(#11525,#11526,#11527,#11528,#11529,
#11530,#11531,#11532,#11533,#11534,#11535),.UNSPECIFIED.,.F.,.F.,(4,1,1,
1,1,1,1,1,4),(28.2743338823083,28.5691616865189,29.5663833623529,30.5636050381868,
31.5608267140208,32.5580483898547,33.5552700656887,34.5524917415226,34.5575191894878),
 .UNSPECIFIED.);
#303=B_SPLINE_CURVE_WITH_KNOTS('',3,(#11536,#11537,#11538,#11539,#11540,
#11541,#11542,#11543,#11544,#11545),.UNSPECIFIED.,.F.,.F.,(4,1,1,1,1,1,
1,4),(28.2743338823083,29.2575833826404,30.2551750805203,31.2527667784002,
32.2503584762801,33.2479501741599,34.2455418720398,34.5575191894879),
 .UNSPECIFIED.);
#304=B_SPLINE_CURVE_WITH_KNOTS('',3,(#11550,#11551,#11552,#11553,#11554,
#11555,#11556,#11557,#11558,#11559),.UNSPECIFIED.,.F.,.F.,(4,1,1,1,1,1,
1,4),(21.9911485751287,22.5858316315152,23.5830533073491,24.5802749831831,
25.577496659017,26.574718334851,27.5719400106849,28.2743338823083),
 .UNSPECIFIED.);
#305=B_SPLINE_CURVE_WITH_KNOTS('',3,(#11560,#11561,#11562,#11563,#11564,
#11565,#11566,#11567,#11568,#11569,#11570),.UNSPECIFIED.,.F.,.F.,(4,1,1,
1,1,1,1,1,4),(21.9911485751287,22.2744414974812,23.2720331953611,24.269624893241,
25.2672165911209,26.2648082890007,27.2623999868806,28.2599916847605,28.2743338823083),
 .UNSPECIFIED.);
#306=B_SPLINE_CURVE_WITH_KNOTS('',3,(#11575,#11576,#11577,#11578,#11579,
#11580,#11581,#11582,#11583,#11584),.UNSPECIFIED.,.F.,.F.,(4,1,1,1,1,1,
1,4),(15.7079632679491,16.6025015765114,17.5997232523454,18.5969449281793,
19.5941666040133,20.5913882798473,21.5886099556812,21.9911485751287),
 .UNSPECIFIED.);
#307=B_SPLINE_CURVE_WITH_KNOTS('',3,(#11585,#11586,#11587,#11588,#11589,
#11590,#11591,#11592,#11593,#11594),.UNSPECIFIED.,.F.,.F.,(4,1,1,1,1,1,
1,4),(15.7079632679491,16.2888913102019,17.2864830080818,18.2840747059617,
19.2816664038415,20.2792581017214,21.2768497996013,21.9911485751287),
 .UNSPECIFIED.);
#308=B_SPLINE_CURVE_WITH_KNOTS('',3,(#11597,#11598,#11599,#11600,#11601,
#11602,#11603,#11604,#11605,#11606,#11607,#11608,#11609,#11610,#11611,#11612,
#11613,#11614,#11615,#11616,#11617,#11618,#11619,#11620,#11621,#11622,#11623,
#11624,#11625,#11626,#11627,#11628,#11629,#11630,#11631,#11632,#11633,#11634,
#11635,#11636,#11637,#11638,#11639,#11640,#11641,#11642,#11643,#11644,#11645,
#11646,#11647,#11648,#11649,#11650,#11651,#11652,#11653,#11654,#11655,#11656,
#11657,#11658,#11659,#11660,#11661,#11662,#11663,#11664,#11665,#11666,#11667,
#11668,#11669,#11670,#11671,#11672,#11673,#11674,#11675,#11676,#11677,#11678,
#11679,#11680,#11681,#11682,#11683,#11684,#11685,#11686,#11687,#11688,#11689,
#11690,#11691,#11692,#11693,#11694,#11695,#11696,#11697,#11698,#11699,#11700,
#11701,#11702,#11703,#11704,#11705,#11706,#11707,#11708,#11709,#11710,#11711,
#11712,#11713,#11714,#11715,#11716,#11717,#11718,#11719,#11720,#11721,#11722,
#11723,#11724,#11725,#11726,#11727,#11728,#11729,#11730,#11731,#11732,#11733,
#11734,#11735,#11736,#11737,#11738,#11739,#11740,#11741,#11742,#11743,#11744,
#11745,#11746,#11747,#11748,#11749,#11750,#11751,#11752,#11753,#11754,#11755,
#11756,#11757,#11758,#11759,#11760,#11761,#11762,#11763,#11764,#11765,#11766,
#11767,#11768,#11769,#11770,#11771,#11772,#11773,#11774,#11775,#11776,#11777,
#11778,#11779,#11780,#11781,#11782,#11783,#11784,#11785,#11786,#11787,#11788,
#11789,#11790,#11791,#11792,#11793,#11794,#11795,#11796,#11797,#11798,#11799,
#11800,#11801,#11802,#11803,#11804,#11805,#11806,#11807,#11808,#11809,#11810),
 .UNSPECIFIED.,.F.,.F.,(4,3,3,3,3,3,3,3,3,3,3,3,3,3,3,3,3,3,3,3,3,3,3,3,
3,3,3,3,3,3,3,3,3,3,3,3,3,3,3,3,3,3,3,3,3,3,3,3,3,3,3,3,3,3,3,3,3,3,3,3,
3,3,3,3,3,3,3,3,3,3,3,4),(-1.26297767193527,-1.24123059946692,-1.21837400953358,
-1.20789928299389,-1.20383483749142,-1.19947717281857,-1.17668714612644,
-1.15373012448748,-1.14469158562245,-1.14082677203282,-1.11762638295685,
-1.0945612252029,-1.07646955260153,-1.0672475154899,-1.06334380101767,-1.05931873640602,
-1.05837788000017,-1.0361298744797,-1.01232110135027,-0.991488424862023,
-0.984594580015151,-0.980621471139353,-0.957200760573628,-0.933467886974511,
-0.91151583759195,-0.903275712213173,-0.898529224186148,-0.895168469288221,
-0.870414079366242,-0.845659689444264,-0.822099707362731,-0.813927294570445,
-0.810210042103504,-0.786549160472357,-0.762432595442628,-0.738225084576931,
-0.729837012816269,-0.725138584726005,-0.700132102528345,-0.675759915730524,
-0.651798333821953,-0.643457982208621,-0.638375085891089,-0.625112655935365,
-0.601401003403345,-0.575798341779257,-0.564089465748533,-0.554431081554694,
-0.550487592904426,-0.525821248520384,-0.500828064063021,-0.474765975649928,
-0.466687959682199,-0.461195933574007,-0.435964800569675,-0.411153539634739,
-0.396579710410647,-0.382859058578158,-0.374421643509067,-0.370946667145629,
-0.346187746128783,-0.320896710423911,-0.29540724904293,-0.285987248141239,
-0.282041885516286,-0.278125401225697,-0.252392678017214,-0.226697892801638,
-0.201873586946231,-0.191255176409111,-0.186426923186837,-0.177049281090825),
 .UNSPECIFIED.);
#309=B_SPLINE_CURVE_WITH_KNOTS('',3,(#11812,#11813,#11814,#11815,#11816,
#11817,#11818,#11819,#11820,#11821,#11822,#11823,#11824,#11825,#11826,#11827,
#11828,#11829,#11830,#11831,#11832,#11833,#11834,#11835,#11836,#11837,#11838,
#11839,#11840,#11841,#11842,#11843,#11844,#11845,#11846,#11847,#11848,#11849,
#11850,#11851,#11852,#11853,#11854,#11855,#11856,#11857,#11858,#11859,#11860,
#11861,#11862,#11863,#11864,#11865,#11866,#11867,#11868,#11869,#11870,#11871,
#11872),.UNSPECIFIED.,.F.,.F.,(4,3,3,3,3,3,3,3,3,3,3,3,3,3,3,3,3,3,3,3,
4),(-0.342658399319032,-0.317027048600994,-0.292003556185365,-0.273617043455568,
-0.259827158908221,-0.255639923465139,-0.231507037422574,-0.218457505266178,
-0.193758751297552,-0.169538907385358,-0.165763510415239,-0.141949579421655,
-0.118190761275412,-0.0948421346464585,-0.0878872820010161,-0.0819188450624042,
-0.0782990769851931,-0.055689554830121,-0.0334445595930238,-0.0118635944753777,
0.),.UNSPECIFIED.);
#310=B_SPLINE_CURVE_WITH_KNOTS('',3,(#11875,#11876,#11877,#11878,#11879,
#11880,#11881,#11882,#11883,#11884,#11885,#11886,#11887,#11888,#11889,#11890,
#11891,#11892,#11893,#11894,#11895,#11896,#11897,#11898,#11899,#11900,#11901,
#11902),.UNSPECIFIED.,.F.,.F.,(4,3,3,3,3,3,3,3,3,4),(-0.177049281090825,
-0.160264958626335,-0.134994935614823,-0.109227006060211,-0.0991214343897917,
-0.0948694657952354,-0.0690591354441416,-0.0428842165991826,-0.0167516322510638,
0.),.UNSPECIFIED.);
#311=B_SPLINE_CURVE_WITH_KNOTS('',3,(#12691,#12692,#12693,#12694,#12695,
#12696,#12697,#12698),.UNSPECIFIED.,.F.,.F.,(4,1,1,1,1,4),(11.6163931973417,
12.6136148731756,13.6108365490096,14.6080582248435,15.6052799006775,15.7079632679491),
 .UNSPECIFIED.);
#312=B_SPLINE_CURVE_WITH_KNOTS('',3,(#12699,#12700,#12701,#12702,#12703,
#12704,#12705,#12706,#12707,#12708,#12709,#12710,#12711,#12712,#12713,#12714,
#12715,#12716,#12717,#12718,#12719,#12720,#12721,#12722,#12723,#12724,#12725,
#12726,#12727,#12728,#12729,#12730,#12731,#12732,#12733,#12734,#12735,#12736,
#12737,#12738,#12739,#12740,#12741,#12742,#12743,#12744,#12745,#12746,#12747,
#12748,#12749,#12750,#12751,#12752,#12753,#12754,#12755,#12756,#12757,#12758,
#12759,#12760,#12761,#12762,#12763,#12764,#12765,#12766,#12767,#12768,#12769,
#12770,#12771,#12772,#12773,#12774,#12775,#12776,#12777,#12778,#12779,#12780,
#12781,#12782,#12783,#12784,#12785,#12786),.UNSPECIFIED.,.F.,.F.,(4,3,3,
3,3,3,3,3,3,3,3,3,3,3,3,3,3,3,3,3,3,3,3,3,3,3,3,3,3,4),(-0.461788964899783,
-0.444143511940815,-0.418515798790508,-0.405575675714164,-0.399737745646638,
-0.394846562641521,-0.369463325133089,-0.349714638187578,-0.340575547651319,
-0.336040482540573,-0.331740177580549,-0.306977516058662,-0.282755448184146,
-0.259069445882197,-0.248566190347295,-0.244441238407051,-0.220951758169334,
-0.211473829568997,-0.187512614410561,-0.164073537609241,-0.158786243270235,
-0.135430453104867,-0.112092295537671,-0.0891436133842281,-0.0803317101641952,
-0.0766176166068317,-0.0541543545622248,-0.0320549846333942,-0.0106630888452865,
0.),.UNSPECIFIED.);
#313=B_SPLINE_CURVE_WITH_KNOTS('',3,(#12787,#12788,#12789,#12790,#12791,
#12792,#12793,#12794,#12795,#12796,#12797,#12798,#12799,#12800,#12801,#12802,
#12803,#12804,#12805),.UNSPECIFIED.,.F.,.F.,(4,3,3,3,3,3,4),(-190.950928956894,
-190.469340084285,-189.472118408451,-188.474896732617,-187.477675056784,
-186.48045338095,-186.303943978815),.UNSPECIFIED.);
#314=B_SPLINE_CURVE_WITH_KNOTS('',3,(#12808,#12809,#12810,#12811,#12812,
#12813,#12814,#12815,#12816),.UNSPECIFIED.,.F.,.F.,(4,1,1,1,1,1,4),(10.3747553777872,
11.3009328208025,12.2985245186824,13.2961162165622,14.2937079144421,15.291299612322,
15.7079632679491),.UNSPECIFIED.);
#315=B_SPLINE_CURVE_WITH_KNOTS('',3,(#13610,#13611,#13612,#13613,#13614,
#13615,#13616,#13617,#13618,#13619,#13620,#13621,#13622,#13623,#13624,#13625,
#13626,#13627,#13628,#13629,#13630,#13631),.UNSPECIFIED.,.F.,.F.,(4,3,3,
3,3,3,3,4),(183.328994141815,183.556872409899,184.554464107779,185.552055805659,
186.549647503538,187.547239201418,188.544830899298,188.88433130627),
 .UNSPECIFIED.);
#316=B_SPLINE_CURVE_WITH_KNOTS('',3,(#13632,#13633,#13634,#13635,#13636,
#13637,#13638,#13639,#13640,#13641,#13642,#13643,#13644,#13645,#13646,#13647,
#13648,#13649,#13650,#13651,#13652,#13653,#13654,#13655,#13656,#13657,#13658,
#13659,#13660,#13661,#13662,#13663,#13664,#13665,#13666,#13667,#13668,#13669,
#13670,#13671,#13672,#13673,#13674,#13675,#13676,#13677,#13678,#13679,#13680,
#13681,#13682,#13683,#13684,#13685,#13686,#13687,#13688,#13689,#13690,#13691,
#13692,#13693,#13694,#13695,#13696,#13697,#13698,#13699,#13700,#13701,#13702,
#13703,#13704,#13705,#13706,#13707,#13708,#13709,#13710,#13711,#13712,#13713,
#13714,#13715,#13716),.UNSPECIFIED.,.F.,.F.,(4,3,3,3,3,3,3,3,3,3,3,3,3,
3,3,3,3,3,3,3,3,3,3,3,3,3,3,3,4),(-0.463803050843705,-0.449347192429686,
-0.427640368714011,-0.415624313505051,-0.410511273392428,-0.406061884229529,
-0.383387971324397,-0.36490408347224,-0.357542028506273,-0.352425153391359,
-0.329101137101116,-0.305332602380306,-0.287878668912014,-0.274788218810795,
-0.271229860207255,-0.246801643139605,-0.235516868507138,-0.211931397815532,
-0.187854419898393,-0.183811601979953,-0.1594364627127,-0.134555356368287,
-0.109447034007667,-0.0941298055661022,-0.0900026856982938,-0.0642548943642791,
-0.0384793716268655,-0.0132580795069667,0.),.UNSPECIFIED.);
#317=SHAPE_REPRESENTATION_RELATIONSHIP('SRR','None',#13835,#323);
#318=SHAPE_REPRESENTATION_RELATIONSHIP('SRR','None',#13836,#324);
#319=SHAPE_REPRESENTATION_RELATIONSHIP('SRR','None',#13837,#325);
#320=SHAPE_REPRESENTATION_RELATIONSHIP('SRR','None',#13838,#326);
#321=SHAPE_REPRESENTATION_RELATIONSHIP('SRR','None',#13839,#327);
#322=SHAPE_REPRESENTATION_RELATIONSHIP('SRR','None',#13840,#328);
#323=ADVANCED_BREP_SHAPE_REPRESENTATION('',(#335),#13795);
#324=ADVANCED_BREP_SHAPE_REPRESENTATION('',(#336),#13796);
#325=ADVANCED_BREP_SHAPE_REPRESENTATION('',(#337),#13797);
#326=ADVANCED_BREP_SHAPE_REPRESENTATION('',(#338),#13798);
#327=ADVANCED_BREP_SHAPE_REPRESENTATION('',(#339),#13799);
#328=ADVANCED_BREP_SHAPE_REPRESENTATION('',(#340),#13800);
#329=STYLED_ITEM('',(#13878),#335);
#330=STYLED_ITEM('',(#13879),#336);
#331=STYLED_ITEM('',(#13880),#337);
#332=STYLED_ITEM('',(#13881),#338);
#333=STYLED_ITEM('',(#13882),#339);
#334=STYLED_ITEM('',(#13883),#340);
#335=MANIFOLD_SOLID_BREP('Body1',#3694);
#336=MANIFOLD_SOLID_BREP('Body1',#3695);
#337=MANIFOLD_SOLID_BREP('Body1',#3696);
#338=MANIFOLD_SOLID_BREP('Body1',#3697);
#339=MANIFOLD_SOLID_BREP('Body1',#3698);
#340=MANIFOLD_SOLID_BREP('Body1',#3699);
#341=FACE_BOUND('',#630,.T.);
#342=FACE_BOUND('',#631,.T.);
#343=FACE_BOUND('',#632,.T.);
#344=FACE_BOUND('',#633,.T.);
#345=FACE_BOUND('',#634,.T.);
#346=FACE_BOUND('',#635,.T.);
#347=FACE_BOUND('',#636,.T.);
#348=FACE_BOUND('',#637,.T.);
#349=FACE_BOUND('',#640,.T.);
#350=FACE_BOUND('',#641,.T.);
#351=FACE_BOUND('',#642,.T.);
#352=FACE_BOUND('',#643,.T.);
#353=FACE_BOUND('',#644,.T.);
#354=FACE_BOUND('',#645,.T.);
#355=FACE_BOUND('',#740,.T.);
#356=FACE_BOUND('',#741,.T.);
#357=FACE_BOUND('',#742,.T.);
#358=FACE_BOUND('',#743,.T.);
#359=FACE_BOUND('',#747,.T.);
#360=FACE_BOUND('',#749,.T.);
#361=FACE_BOUND('',#759,.T.);
#362=FACE_BOUND('',#761,.T.);
#363=FACE_BOUND('',#835,.T.);
#364=FACE_BOUND('',#838,.T.);
#365=PLANE('',#3773);
#366=PLANE('',#3777);
#367=PLANE('',#3796);
#368=PLANE('',#3797);
#369=PLANE('',#3798);
#370=PLANE('',#3799);
#371=PLANE('',#3800);
#372=PLANE('',#3801);
#373=PLANE('',#3870);
#374=PLANE('',#3874);
#375=PLANE('',#3875);
#376=PLANE('',#3878);
#377=PLANE('',#3881);
#378=PLANE('',#3882);
#379=PLANE('',#3883);
#380=PLANE('',#3887);
#381=PLANE('',#3891);
#382=PLANE('',#3895);
#383=PLANE('',#3902);
#384=PLANE('',#3906);
#385=PLANE('',#3907);
#386=PLANE('',#3908);
#387=PLANE('',#3909);
#388=PLANE('',#3910);
#389=PLANE('',#3914);
#390=PLANE('',#3918);
#391=PLANE('',#3919);
#392=PLANE('',#3920);
#393=PLANE('',#3921);
#394=PLANE('',#3922);
#395=PLANE('',#3923);
#396=PLANE('',#3924);
#397=PLANE('',#3926);
#398=PLANE('',#3927);
#399=PLANE('',#3928);
#400=PLANE('',#3929);
#401=PLANE('',#3930);
#402=PLANE('',#3931);
#403=PLANE('',#3939);
#404=PLANE('',#3940);
#405=PLANE('',#4010);
#406=PLANE('',#4011);
#407=PLANE('',#4012);
#408=PLANE('',#4013);
#409=PLANE('',#4014);
#410=PLANE('',#4015);
#411=PLANE('',#4016);
#412=PLANE('',#4017);
#413=PLANE('',#4021);
#414=PLANE('',#4022);
#415=PLANE('',#4027);
#416=PLANE('',#4028);
#417=FACE_OUTER_BOUND('',#618,.T.);
#418=FACE_OUTER_BOUND('',#619,.T.);
#419=FACE_OUTER_BOUND('',#620,.T.);
#420=FACE_OUTER_BOUND('',#621,.T.);
#421=FACE_OUTER_BOUND('',#622,.T.);
#422=FACE_OUTER_BOUND('',#623,.T.);
#423=FACE_OUTER_BOUND('',#624,.T.);
#424=FACE_OUTER_BOUND('',#625,.T.);
#425=FACE_OUTER_BOUND('',#626,.T.);
#426=FACE_OUTER_BOUND('',#627,.T.);
#427=FACE_OUTER_BOUND('',#628,.T.);
#428=FACE_OUTER_BOUND('',#629,.T.);
#429=FACE_OUTER_BOUND('',#638,.T.);
#430=FACE_OUTER_BOUND('',#639,.T.);
#431=FACE_OUTER_BOUND('',#646,.T.);
#432=FACE_OUTER_BOUND('',#647,.T.);
#433=FACE_OUTER_BOUND('',#648,.T.);
#434=FACE_OUTER_BOUND('',#649,.T.);
#435=FACE_OUTER_BOUND('',#650,.T.);
#436=FACE_OUTER_BOUND('',#651,.T.);
#437=FACE_OUTER_BOUND('',#652,.T.);
#438=FACE_OUTER_BOUND('',#653,.T.);
#439=FACE_OUTER_BOUND('',#654,.T.);
#440=FACE_OUTER_BOUND('',#655,.T.);
#441=FACE_OUTER_BOUND('',#656,.T.);
#442=FACE_OUTER_BOUND('',#657,.T.);
#443=FACE_OUTER_BOUND('',#658,.T.);
#444=FACE_OUTER_BOUND('',#659,.T.);
#445=FACE_OUTER_BOUND('',#660,.T.);
#446=FACE_OUTER_BOUND('',#661,.T.);
#447=FACE_OUTER_BOUND('',#662,.T.);
#448=FACE_OUTER_BOUND('',#663,.T.);
#449=FACE_OUTER_BOUND('',#664,.T.);
#450=FACE_OUTER_BOUND('',#665,.T.);
#451=FACE_OUTER_BOUND('',#666,.T.);
#452=FACE_OUTER_BOUND('',#667,.T.);
#453=FACE_OUTER_BOUND('',#668,.T.);
#454=FACE_OUTER_BOUND('',#669,.T.);
#455=FACE_OUTER_BOUND('',#670,.T.);
#456=FACE_OUTER_BOUND('',#671,.T.);
#457=FACE_OUTER_BOUND('',#672,.T.);
#458=FACE_OUTER_BOUND('',#673,.T.);
#459=FACE_OUTER_BOUND('',#674,.T.);
#460=FACE_OUTER_BOUND('',#675,.T.);
#461=FACE_OUTER_BOUND('',#676,.T.);
#462=FACE_OUTER_BOUND('',#677,.T.);
#463=FACE_OUTER_BOUND('',#678,.T.);
#464=FACE_OUTER_BOUND('',#679,.T.);
#465=FACE_OUTER_BOUND('',#680,.T.);
#466=FACE_OUTER_BOUND('',#681,.T.);
#467=FACE_OUTER_BOUND('',#682,.T.);
#468=FACE_OUTER_BOUND('',#683,.T.);
#469=FACE_OUTER_BOUND('',#684,.T.);
#470=FACE_OUTER_BOUND('',#685,.T.);
#471=FACE_OUTER_BOUND('',#686,.T.);
#472=FACE_OUTER_BOUND('',#687,.T.);
#473=FACE_OUTER_BOUND('',#688,.T.);
#474=FACE_OUTER_BOUND('',#689,.T.);
#475=FACE_OUTER_BOUND('',#690,.T.);
#476=FACE_OUTER_BOUND('',#691,.T.);
#477=FACE_OUTER_BOUND('',#692,.T.);
#478=FACE_OUTER_BOUND('',#693,.T.);
#479=FACE_OUTER_BOUND('',#694,.T.);
#480=FACE_OUTER_BOUND('',#695,.T.);
#481=FACE_OUTER_BOUND('',#696,.T.);
#482=FACE_OUTER_BOUND('',#697,.T.);
#483=FACE_OUTER_BOUND('',#698,.T.);
#484=FACE_OUTER_BOUND('',#699,.T.);
#485=FACE_OUTER_BOUND('',#700,.T.);
#486=FACE_OUTER_BOUND('',#701,.T.);
#487=FACE_OUTER_BOUND('',#702,.T.);
#488=FACE_OUTER_BOUND('',#703,.T.);
#489=FACE_OUTER_BOUND('',#704,.T.);
#490=FACE_OUTER_BOUND('',#705,.T.);
#491=FACE_OUTER_BOUND('',#706,.T.);
#492=FACE_OUTER_BOUND('',#707,.T.);
#493=FACE_OUTER_BOUND('',#708,.T.);
#494=FACE_OUTER_BOUND('',#709,.T.);
#495=FACE_OUTER_BOUND('',#710,.T.);
#496=FACE_OUTER_BOUND('',#711,.T.);
#497=FACE_OUTER_BOUND('',#712,.T.);
#498=FACE_OUTER_BOUND('',#713,.T.);
#499=FACE_OUTER_BOUND('',#714,.T.);
#500=FACE_OUTER_BOUND('',#715,.T.);
#501=FACE_OUTER_BOUND('',#716,.T.);
#502=FACE_OUTER_BOUND('',#717,.T.);
#503=FACE_OUTER_BOUND('',#718,.T.);
#504=FACE_OUTER_BOUND('',#719,.T.);
#505=FACE_OUTER_BOUND('',#720,.T.);
#506=FACE_OUTER_BOUND('',#721,.T.);
#507=FACE_OUTER_BOUND('',#722,.T.);
#508=FACE_OUTER_BOUND('',#723,.T.);
#509=FACE_OUTER_BOUND('',#724,.T.);
#510=FACE_OUTER_BOUND('',#725,.T.);
#511=FACE_OUTER_BOUND('',#726,.T.);
#512=FACE_OUTER_BOUND('',#727,.T.);
#513=FACE_OUTER_BOUND('',#728,.T.);
#514=FACE_OUTER_BOUND('',#729,.T.);
#515=FACE_OUTER_BOUND('',#730,.T.);
#516=FACE_OUTER_BOUND('',#731,.T.);
#517=FACE_OUTER_BOUND('',#732,.T.);
#518=FACE_OUTER_BOUND('',#733,.T.);
#519=FACE_OUTER_BOUND('',#734,.T.);
#520=FACE_OUTER_BOUND('',#735,.T.);
#521=FACE_OUTER_BOUND('',#736,.T.);
#522=FACE_OUTER_BOUND('',#737,.T.);
#523=FACE_OUTER_BOUND('',#738,.T.);
#524=FACE_OUTER_BOUND('',#739,.T.);
#525=FACE_OUTER_BOUND('',#744,.T.);
#526=FACE_OUTER_BOUND('',#745,.T.);
#527=FACE_OUTER_BOUND('',#746,.T.);
#528=FACE_OUTER_BOUND('',#748,.T.);
#529=FACE_OUTER_BOUND('',#750,.T.);
#530=FACE_OUTER_BOUND('',#751,.T.);
#531=FACE_OUTER_BOUND('',#752,.T.);
#532=FACE_OUTER_BOUND('',#753,.T.);
#533=FACE_OUTER_BOUND('',#754,.T.);
#534=FACE_OUTER_BOUND('',#755,.T.);
#535=FACE_OUTER_BOUND('',#756,.T.);
#536=FACE_OUTER_BOUND('',#757,.T.);
#537=FACE_OUTER_BOUND('',#758,.T.);
#538=FACE_OUTER_BOUND('',#760,.T.);
#539=FACE_OUTER_BOUND('',#762,.T.);
#540=FACE_OUTER_BOUND('',#763,.T.);
#541=FACE_OUTER_BOUND('',#764,.T.);
#542=FACE_OUTER_BOUND('',#765,.T.);
#543=FACE_OUTER_BOUND('',#766,.T.);
#544=FACE_OUTER_BOUND('',#767,.T.);
#545=FACE_OUTER_BOUND('',#768,.T.);
#546=FACE_OUTER_BOUND('',#769,.T.);
#547=FACE_OUTER_BOUND('',#770,.T.);
#548=FACE_OUTER_BOUND('',#771,.T.);
#549=FACE_OUTER_BOUND('',#772,.T.);
#550=FACE_OUTER_BOUND('',#773,.T.);
#551=FACE_OUTER_BOUND('',#774,.T.);
#552=FACE_OUTER_BOUND('',#775,.T.);
#553=FACE_OUTER_BOUND('',#776,.T.);
#554=FACE_OUTER_BOUND('',#777,.T.);
#555=FACE_OUTER_BOUND('',#778,.T.);
#556=FACE_OUTER_BOUND('',#779,.T.);
#557=FACE_OUTER_BOUND('',#780,.T.);
#558=FACE_OUTER_BOUND('',#781,.T.);
#559=FACE_OUTER_BOUND('',#782,.T.);
#560=FACE_OUTER_BOUND('',#783,.T.);
#561=FACE_OUTER_BOUND('',#784,.T.);
#562=FACE_OUTER_BOUND('',#785,.T.);
#563=FACE_OUTER_BOUND('',#786,.T.);
#564=FACE_OUTER_BOUND('',#787,.T.);
#565=FACE_OUTER_BOUND('',#788,.T.);
#566=FACE_OUTER_BOUND('',#789,.T.);
#567=FACE_OUTER_BOUND('',#790,.T.);
#568=FACE_OUTER_BOUND('',#791,.T.);
#569=FACE_OUTER_BOUND('',#792,.T.);
#570=FACE_OUTER_BOUND('',#793,.T.);
#571=FACE_OUTER_BOUND('',#794,.T.);
#572=FACE_OUTER_BOUND('',#795,.T.);
#573=FACE_OUTER_BOUND('',#796,.T.);
#574=FACE_OUTER_BOUND('',#797,.T.);
#575=FACE_OUTER_BOUND('',#798,.T.);
#576=FACE_OUTER_BOUND('',#799,.T.);
#577=FACE_OUTER_BOUND('',#800,.T.);
#578=FACE_OUTER_BOUND('',#801,.T.);
#579=FACE_OUTER_BOUND('',#802,.T.);
#580=FACE_OUTER_BOUND('',#803,.T.);
#581=FACE_OUTER_BOUND('',#804,.T.);
#582=FACE_OUTER_BOUND('',#805,.T.);
#583=FACE_OUTER_BOUND('',#806,.T.);
#584=FACE_OUTER_BOUND('',#807,.T.);
#585=FACE_OUTER_BOUND('',#808,.T.);
#586=FACE_OUTER_BOUND('',#809,.T.);
#587=FACE_OUTER_BOUND('',#810,.T.);
#588=FACE_OUTER_BOUND('',#811,.T.);
#589=FACE_OUTER_BOUND('',#812,.T.);
#590=FACE_OUTER_BOUND('',#813,.T.);
#591=FACE_OUTER_BOUND('',#814,.T.);
#592=FACE_OUTER_BOUND('',#815,.T.);
#593=FACE_OUTER_BOUND('',#816,.T.);
#594=FACE_OUTER_BOUND('',#817,.T.);
#595=FACE_OUTER_BOUND('',#818,.T.);
#596=FACE_OUTER_BOUND('',#819,.T.);
#597=FACE_OUTER_BOUND('',#820,.T.);
#598=FACE_OUTER_BOUND('',#821,.T.);
#599=FACE_OUTER_BOUND('',#822,.T.);
#600=FACE_OUTER_BOUND('',#823,.T.);
#601=FACE_OUTER_BOUND('',#824,.T.);
#602=FACE_OUTER_BOUND('',#825,.T.);
#603=FACE_OUTER_BOUND('',#826,.T.);
#604=FACE_OUTER_BOUND('',#827,.T.);
#605=FACE_OUTER_BOUND('',#828,.T.);
#606=FACE_OUTER_BOUND('',#829,.T.);
#607=FACE_OUTER_BOUND('',#830,.T.);
#608=FACE_OUTER_BOUND('',#831,.T.);
#609=FACE_OUTER_BOUND('',#832,.T.);
#610=FACE_OUTER_BOUND('',#833,.T.);
#611=FACE_OUTER_BOUND('',#834,.T.);
#612=FACE_OUTER_BOUND('',#836,.T.);
#613=FACE_OUTER_BOUND('',#837,.T.);
#614=FACE_OUTER_BOUND('',#839,.T.);
#615=FACE_OUTER_BOUND('',#840,.T.);
#616=FACE_OUTER_BOUND('',#841,.T.);
#617=FACE_OUTER_BOUND('',#842,.T.);
#618=EDGE_LOOP('',(#2265,#2266,#2267,#2268));
#619=EDGE_LOOP('',(#2269));
#620=EDGE_LOOP('',(#2270,#2271,#2272,#2273));
#621=EDGE_LOOP('',(#2274));
#622=EDGE_LOOP('',(#2275,#2276,#2277,#2278));
#623=EDGE_LOOP('',(#2279,#2280,#2281,#2282));
#624=EDGE_LOOP('',(#2283,#2284,#2285,#2286));
#625=EDGE_LOOP('',(#2287,#2288,#2289,#2290));
#626=EDGE_LOOP('',(#2291,#2292,#2293,#2294));
#627=EDGE_LOOP('',(#2295,#2296,#2297,#2298));
#628=EDGE_LOOP('',(#2299,#2300,#2301,#2302));
#629=EDGE_LOOP('',(#2303,#2304,#2305,#2306));
#630=EDGE_LOOP('',(#2307));
#631=EDGE_LOOP('',(#2308));
#632=EDGE_LOOP('',(#2309));
#633=EDGE_LOOP('',(#2310));
#634=EDGE_LOOP('',(#2311));
#635=EDGE_LOOP('',(#2312));
#636=EDGE_LOOP('',(#2313));
#637=EDGE_LOOP('',(#2314));
#638=EDGE_LOOP('',(#2315,#2316,#2317,#2318));
#639=EDGE_LOOP('',(#2319,#2320,#2321,#2322));
#640=EDGE_LOOP('',(#2323));
#641=EDGE_LOOP('',(#2324));
#642=EDGE_LOOP('',(#2325));
#643=EDGE_LOOP('',(#2326));
#644=EDGE_LOOP('',(#2327));
#645=EDGE_LOOP('',(#2328));
#646=EDGE_LOOP('',(#2329,#2330,#2331,#2332));
#647=EDGE_LOOP('',(#2333,#2334,#2335,#2336));
#648=EDGE_LOOP('',(#2337,#2338,#2339,#2340,#2341,#2342,#2343,#2344));
#649=EDGE_LOOP('',(#2345,#2346,#2347,#2348));
#650=EDGE_LOOP('',(#2349,#2350,#2351,#2352));
#651=EDGE_LOOP('',(#2353,#2354,#2355,#2356));
#652=EDGE_LOOP('',(#2357,#2358,#2359,#2360));
#653=EDGE_LOOP('',(#2361,#2362,#2363,#2364));
#654=EDGE_LOOP('',(#2365,#2366,#2367,#2368));
#655=EDGE_LOOP('',(#2369,#2370,#2371,#2372));
#656=EDGE_LOOP('',(#2373,#2374,#2375,#2376));
#657=EDGE_LOOP('',(#2377,#2378,#2379,#2380));
#658=EDGE_LOOP('',(#2381,#2382,#2383,#2384));
#659=EDGE_LOOP('',(#2385,#2386,#2387,#2388));
#660=EDGE_LOOP('',(#2389,#2390,#2391,#2392));
#661=EDGE_LOOP('',(#2393,#2394,#2395,#2396));
#662=EDGE_LOOP('',(#2397,#2398,#2399,#2400));
#663=EDGE_LOOP('',(#2401,#2402,#2403,#2404));
#664=EDGE_LOOP('',(#2405,#2406,#2407,#2408));
#665=EDGE_LOOP('',(#2409,#2410,#2411,#2412));
#666=EDGE_LOOP('',(#2413,#2414,#2415,#2416));
#667=EDGE_LOOP('',(#2417,#2418,#2419,#2420));
#668=EDGE_LOOP('',(#2421,#2422,#2423,#2424));
#669=EDGE_LOOP('',(#2425,#2426,#2427,#2428));
#670=EDGE_LOOP('',(#2429,#2430,#2431,#2432));
#671=EDGE_LOOP('',(#2433,#2434,#2435,#2436));
#672=EDGE_LOOP('',(#2437,#2438,#2439,#2440));
#673=EDGE_LOOP('',(#2441,#2442,#2443,#2444));
#674=EDGE_LOOP('',(#2445,#2446,#2447,#2448));
#675=EDGE_LOOP('',(#2449,#2450,#2451,#2452,#2453,#2454,#2455,#2456));
#676=EDGE_LOOP('',(#2457,#2458,#2459,#2460));
#677=EDGE_LOOP('',(#2461,#2462,#2463,#2464));
#678=EDGE_LOOP('',(#2465,#2466,#2467,#2468));
#679=EDGE_LOOP('',(#2469,#2470,#2471,#2472));
#680=EDGE_LOOP('',(#2473,#2474,#2475,#2476));
#681=EDGE_LOOP('',(#2477,#2478,#2479,#2480));
#682=EDGE_LOOP('',(#2481,#2482,#2483,#2484));
#683=EDGE_LOOP('',(#2485,#2486,#2487,#2488));
#684=EDGE_LOOP('',(#2489,#2490,#2491,#2492));
#685=EDGE_LOOP('',(#2493,#2494,#2495,#2496));
#686=EDGE_LOOP('',(#2497,#2498,#2499,#2500));
#687=EDGE_LOOP('',(#2501,#2502,#2503,#2504));
#688=EDGE_LOOP('',(#2505,#2506,#2507,#2508));
#689=EDGE_LOOP('',(#2509,#2510,#2511,#2512));
#690=EDGE_LOOP('',(#2513,#2514,#2515,#2516));
#691=EDGE_LOOP('',(#2517,#2518,#2519,#2520));
#692=EDGE_LOOP('',(#2521,#2522,#2523,#2524));
#693=EDGE_LOOP('',(#2525,#2526,#2527,#2528));
#694=EDGE_LOOP('',(#2529,#2530,#2531,#2532));
#695=EDGE_LOOP('',(#2533,#2534,#2535,#2536));
#696=EDGE_LOOP('',(#2537,#2538,#2539,#2540));
#697=EDGE_LOOP('',(#2541,#2542,#2543,#2544));
#698=EDGE_LOOP('',(#2545,#2546,#2547,#2548));
#699=EDGE_LOOP('',(#2549,#2550,#2551,#2552));
#700=EDGE_LOOP('',(#2553,#2554,#2555,#2556));
#701=EDGE_LOOP('',(#2557,#2558,#2559,#2560));
#702=EDGE_LOOP('',(#2561,#2562,#2563,#2564));
#703=EDGE_LOOP('',(#2565));
#704=EDGE_LOOP('',(#2566,#2567,#2568,#2569));
#705=EDGE_LOOP('',(#2570));
#706=EDGE_LOOP('',(#2571,#2572,#2573,#2574));
#707=EDGE_LOOP('',(#2575,#2576,#2577,#2578));
#708=EDGE_LOOP('',(#2579,#2580,#2581,#2582,#2583,#2584,#2585,#2586,#2587,
#2588,#2589,#2590,#2591,#2592,#2593,#2594,#2595,#2596,#2597,#2598,#2599,
#2600,#2601,#2602,#2603,#2604,#2605,#2606,#2607,#2608,#2609,#2610));
#709=EDGE_LOOP('',(#2611,#2612,#2613,#2614,#2615,#2616,#2617,#2618,#2619,
#2620,#2621,#2622,#2623,#2624,#2625,#2626,#2627,#2628,#2629,#2630,#2631,
#2632,#2633,#2634,#2635,#2636,#2637,#2638,#2639,#2640,#2641));
#710=EDGE_LOOP('',(#2642,#2643,#2644,#2645));
#711=EDGE_LOOP('',(#2646,#2647,#2648,#2649));
#712=EDGE_LOOP('',(#2650,#2651,#2652,#2653));
#713=EDGE_LOOP('',(#2654,#2655,#2656,#2657,#2658,#2659,#2660,#2661,#2662,
#2663,#2664,#2665,#2666,#2667,#2668,#2669,#2670,#2671,#2672,#2673,#2674,
#2675,#2676,#2677,#2678,#2679,#2680,#2681,#2682,#2683,#2684,#2685));
#714=EDGE_LOOP('',(#2686,#2687,#2688,#2689,#2690,#2691,#2692,#2693,#2694,
#2695,#2696,#2697,#2698,#2699,#2700,#2701,#2702,#2703,#2704,#2705,#2706,
#2707,#2708,#2709,#2710,#2711,#2712,#2713,#2714,#2715,#2716));
#715=EDGE_LOOP('',(#2717,#2718,#2719,#2720));
#716=EDGE_LOOP('',(#2721));
#717=EDGE_LOOP('',(#2722));
#718=EDGE_LOOP('',(#2723,#2724,#2725,#2726));
#719=EDGE_LOOP('',(#2727,#2728,#2729,#2730));
#720=EDGE_LOOP('',(#2731,#2732,#2733,#2734));
#721=EDGE_LOOP('',(#2735,#2736,#2737,#2738));
#722=EDGE_LOOP('',(#2739,#2740,#2741,#2742));
#723=EDGE_LOOP('',(#2743,#2744,#2745,#2746));
#724=EDGE_LOOP('',(#2747,#2748,#2749,#2750));
#725=EDGE_LOOP('',(#2751,#2752,#2753,#2754));
#726=EDGE_LOOP('',(#2755,#2756,#2757,#2758));
#727=EDGE_LOOP('',(#2759,#2760,#2761,#2762));
#728=EDGE_LOOP('',(#2763,#2764,#2765,#2766));
#729=EDGE_LOOP('',(#2767,#2768,#2769,#2770));
#730=EDGE_LOOP('',(#2771,#2772,#2773,#2774));
#731=EDGE_LOOP('',(#2775,#2776,#2777,#2778));
#732=EDGE_LOOP('',(#2779,#2780,#2781,#2782));
#733=EDGE_LOOP('',(#2783,#2784,#2785,#2786));
#734=EDGE_LOOP('',(#2787,#2788,#2789,#2790));
#735=EDGE_LOOP('',(#2791,#2792,#2793,#2794));
#736=EDGE_LOOP('',(#2795,#2796,#2797,#2798));
#737=EDGE_LOOP('',(#2799,#2800,#2801,#2802));
#738=EDGE_LOOP('',(#2803,#2804,#2805,#2806));
#739=EDGE_LOOP('',(#2807,#2808,#2809,#2810));
#740=EDGE_LOOP('',(#2811));
#741=EDGE_LOOP('',(#2812));
#742=EDGE_LOOP('',(#2813,#2814,#2815,#2816));
#743=EDGE_LOOP('',(#2817,#2818,#2819,#2820));
#744=EDGE_LOOP('',(#2821,#2822,#2823,#2824));
#745=EDGE_LOOP('',(#2825,#2826,#2827,#2828));
#746=EDGE_LOOP('',(#2829,#2830,#2831,#2832,#2833,#2834,#2835,#2836,#2837,
#2838,#2839,#2840,#2841,#2842,#2843,#2844));
#747=EDGE_LOOP('',(#2845,#2846,#2847,#2848,#2849,#2850,#2851,#2852));
#748=EDGE_LOOP('',(#2853,#2854,#2855,#2856,#2857,#2858,#2859,#2860,#2861,
#2862,#2863,#2864,#2865,#2866,#2867,#2868));
#749=EDGE_LOOP('',(#2869,#2870,#2871,#2872,#2873,#2874,#2875,#2876));
#750=EDGE_LOOP('',(#2877,#2878,#2879,#2880));
#751=EDGE_LOOP('',(#2881,#2882,#2883,#2884));
#752=EDGE_LOOP('',(#2885,#2886,#2887,#2888));
#753=EDGE_LOOP('',(#2889,#2890,#2891,#2892));
#754=EDGE_LOOP('',(#2893,#2894,#2895,#2896));
#755=EDGE_LOOP('',(#2897,#2898,#2899,#2900));
#756=EDGE_LOOP('',(#2901,#2902,#2903,#2904));
#757=EDGE_LOOP('',(#2905,#2906,#2907,#2908));
#758=EDGE_LOOP('',(#2909));
#759=EDGE_LOOP('',(#2910));
#760=EDGE_LOOP('',(#2911));
#761=EDGE_LOOP('',(#2912));
#762=EDGE_LOOP('',(#2913,#2914,#2915,#2916));
#763=EDGE_LOOP('',(#2917,#2918,#2919,#2920));
#764=EDGE_LOOP('',(#2921,#2922,#2923,#2924));
#765=EDGE_LOOP('',(#2925,#2926,#2927,#2928));
#766=EDGE_LOOP('',(#2929,#2930,#2931,#2932));
#767=EDGE_LOOP('',(#2933,#2934,#2935,#2936));
#768=EDGE_LOOP('',(#2937,#2938,#2939,#2940));
#769=EDGE_LOOP('',(#2941,#2942,#2943,#2944));
#770=EDGE_LOOP('',(#2945,#2946,#2947,#2948));
#771=EDGE_LOOP('',(#2949,#2950,#2951,#2952));
#772=EDGE_LOOP('',(#2953,#2954,#2955,#2956));
#773=EDGE_LOOP('',(#2957,#2958,#2959,#2960));
#774=EDGE_LOOP('',(#2961,#2962,#2963,#2964));
#775=EDGE_LOOP('',(#2965,#2966,#2967,#2968));
#776=EDGE_LOOP('',(#2969,#2970,#2971,#2972));
#777=EDGE_LOOP('',(#2973,#2974,#2975,#2976));
#778=EDGE_LOOP('',(#2977,#2978,#2979,#2980));
#779=EDGE_LOOP('',(#2981,#2982,#2983,#2984));
#780=EDGE_LOOP('',(#2985,#2986,#2987,#2988));
#781=EDGE_LOOP('',(#2989,#2990,#2991,#2992));
#782=EDGE_LOOP('',(#2993,#2994,#2995,#2996));
#783=EDGE_LOOP('',(#2997,#2998,#2999,#3000));
#784=EDGE_LOOP('',(#3001,#3002,#3003,#3004));
#785=EDGE_LOOP('',(#3005,#3006,#3007,#3008));
#786=EDGE_LOOP('',(#3009,#3010,#3011,#3012));
#787=EDGE_LOOP('',(#3013,#3014,#3015,#3016));
#788=EDGE_LOOP('',(#3017,#3018,#3019,#3020));
#789=EDGE_LOOP('',(#3021,#3022,#3023,#3024));
#790=EDGE_LOOP('',(#3025,#3026,#3027,#3028));
#791=EDGE_LOOP('',(#3029,#3030,#3031,#3032));
#792=EDGE_LOOP('',(#3033,#3034,#3035,#3036));
#793=EDGE_LOOP('',(#3037,#3038,#3039,#3040));
#794=EDGE_LOOP('',(#3041,#3042,#3043,#3044));
#795=EDGE_LOOP('',(#3045,#3046,#3047,#3048));
#796=EDGE_LOOP('',(#3049,#3050,#3051,#3052));
#797=EDGE_LOOP('',(#3053,#3054,#3055,#3056));
#798=EDGE_LOOP('',(#3057,#3058,#3059,#3060));
#799=EDGE_LOOP('',(#3061,#3062,#3063,#3064));
#800=EDGE_LOOP('',(#3065,#3066,#3067,#3068));
#801=EDGE_LOOP('',(#3069,#3070,#3071,#3072));
#802=EDGE_LOOP('',(#3073,#3074,#3075,#3076));
#803=EDGE_LOOP('',(#3077,#3078,#3079,#3080));
#804=EDGE_LOOP('',(#3081,#3082,#3083,#3084));
#805=EDGE_LOOP('',(#3085,#3086,#3087,#3088));
#806=EDGE_LOOP('',(#3089,#3090,#3091,#3092));
#807=EDGE_LOOP('',(#3093,#3094,#3095,#3096));
#808=EDGE_LOOP('',(#3097,#3098,#3099,#3100));
#809=EDGE_LOOP('',(#3101,#3102,#3103,#3104));
#810=EDGE_LOOP('',(#3105,#3106,#3107,#3108));
#811=EDGE_LOOP('',(#3109,#3110,#3111,#3112));
#812=EDGE_LOOP('',(#3113,#3114,#3115,#3116));
#813=EDGE_LOOP('',(#3117,#3118,#3119,#3120));
#814=EDGE_LOOP('',(#3121,#3122,#3123,#3124));
#815=EDGE_LOOP('',(#3125,#3126,#3127,#3128));
#816=EDGE_LOOP('',(#3129,#3130,#3131,#3132));
#817=EDGE_LOOP('',(#3133,#3134,#3135,#3136));
#818=EDGE_LOOP('',(#3137,#3138,#3139,#3140));
#819=EDGE_LOOP('',(#3141,#3142,#3143,#3144));
#820=EDGE_LOOP('',(#3145,#3146,#3147,#3148));
#821=EDGE_LOOP('',(#3149,#3150,#3151,#3152));
#822=EDGE_LOOP('',(#3153,#3154,#3155,#3156,#3157,#3158,#3159,#3160));
#823=EDGE_LOOP('',(#3161,#3162,#3163,#3164,#3165,#3166,#3167,#3168,#3169,
#3170,#3171,#3172,#3173,#3174,#3175,#3176,#3177,#3178,#3179,#3180,#3181,
#3182,#3183,#3184,#3185,#3186,#3187,#3188,#3189,#3190,#3191,#3192,#3193,
#3194,#3195,#3196,#3197,#3198,#3199,#3200,#3201,#3202,#3203,#3204,#3205,
#3206,#3207,#3208,#3209,#3210,#3211,#3212,#3213,#3214,#3215,#3216,#3217,
#3218,#3219,#3220,#3221,#3222,#3223,#3224));
#824=EDGE_LOOP('',(#3225,#3226,#3227,#3228));
#825=EDGE_LOOP('',(#3229,#3230,#3231,#3232,#3233,#3234,#3235,#3236,#3237,
#3238,#3239,#3240,#3241,#3242,#3243,#3244,#3245,#3246,#3247,#3248,#3249,
#3250,#3251,#3252,#3253,#3254,#3255,#3256,#3257,#3258,#3259,#3260,#3261,
#3262,#3263,#3264,#3265,#3266,#3267,#3268,#3269,#3270,#3271,#3272,#3273,
#3274,#3275,#3276,#3277,#3278,#3279,#3280,#3281,#3282,#3283,#3284,#3285,
#3286,#3287,#3288,#3289,#3290,#3291,#3292,#3293));
#826=EDGE_LOOP('',(#3294,#3295,#3296,#3297));
#827=EDGE_LOOP('',(#3298,#3299,#3300,#3301));
#828=EDGE_LOOP('',(#3302,#3303,#3304,#3305));
#829=EDGE_LOOP('',(#3306,#3307,#3308,#3309));
#830=EDGE_LOOP('',(#3310,#3311,#3312,#3313));
#831=EDGE_LOOP('',(#3314,#3315,#3316,#3317));
#832=EDGE_LOOP('',(#3318,#3319,#3320,#3321));
#833=EDGE_LOOP('',(#3322,#3323,#3324,#3325,#3326,#3327));
#834=EDGE_LOOP('',(#3328));
#835=EDGE_LOOP('',(#3329,#3330,#3331,#3332));
#836=EDGE_LOOP('',(#3333,#3334,#3335,#3336));
#837=EDGE_LOOP('',(#3337));
#838=EDGE_LOOP('',(#3338,#3339,#3340,#3341,#3342,#3343));
#839=EDGE_LOOP('',(#3344));
#840=EDGE_LOOP('',(#3345,#3346,#3347,#3348));
#841=EDGE_LOOP('',(#3349));
#842=EDGE_LOOP('',(#3350));
#843=LINE('',#4822,#1072);
#844=LINE('',#4829,#1073);
#845=LINE('',#4836,#1074);
#846=LINE('',#4842,#1075);
#847=LINE('',#4848,#1076);
#848=LINE('',#4854,#1077);
#849=LINE('',#4860,#1078);
#850=LINE('',#4866,#1079);
#851=LINE('',#4871,#1080);
#852=LINE('',#4873,#1081);
#853=LINE('',#4875,#1082);
#854=LINE('',#4876,#1083);
#855=LINE('',#4879,#1084);
#856=LINE('',#4881,#1085);
#857=LINE('',#4882,#1086);
#858=LINE('',#4885,#1087);
#859=LINE('',#4887,#1088);
#860=LINE('',#4888,#1089);
#861=LINE('',#4890,#1090);
#862=LINE('',#4891,#1091);
#863=LINE('',#4898,#1092);
#864=LINE('',#4927,#1093);
#865=LINE('',#4957,#1094);
#866=LINE('',#5005,#1095);
#867=LINE('',#5056,#1096);
#868=LINE('',#5107,#1097);
#869=LINE('',#5155,#1098);
#870=LINE('',#5206,#1099);
#871=LINE('',#5257,#1100);
#872=LINE('',#5305,#1101);
#873=LINE('',#5356,#1102);
#874=LINE('',#5407,#1103);
#875=LINE('',#5455,#1104);
#876=LINE('',#5506,#1105);
#877=LINE('',#5545,#1106);
#878=LINE('',#5565,#1107);
#879=LINE('',#5590,#1108);
#880=LINE('',#5615,#1109);
#881=LINE('',#5639,#1110);
#882=LINE('',#5664,#1111);
#883=LINE('',#5689,#1112);
#884=LINE('',#5713,#1113);
#885=LINE('',#5738,#1114);
#886=LINE('',#5763,#1115);
#887=LINE('',#5787,#1116);
#888=LINE('',#5812,#1117);
#889=LINE('',#5837,#1118);
#890=LINE('',#5861,#1119);
#891=LINE('',#5878,#1120);
#892=LINE('',#5907,#1121);
#893=LINE('',#5937,#1122);
#894=LINE('',#5985,#1123);
#895=LINE('',#6036,#1124);
#896=LINE('',#6087,#1125);
#897=LINE('',#6135,#1126);
#898=LINE('',#6186,#1127);
#899=LINE('',#6237,#1128);
#900=LINE('',#6285,#1129);
#901=LINE('',#6336,#1130);
#902=LINE('',#6387,#1131);
#903=LINE('',#6435,#1132);
#904=LINE('',#6486,#1133);
#905=LINE('',#6525,#1134);
#906=LINE('',#6545,#1135);
#907=LINE('',#6570,#1136);
#908=LINE('',#6595,#1137);
#909=LINE('',#6619,#1138);
#910=LINE('',#6644,#1139);
#911=LINE('',#6669,#1140);
#912=LINE('',#6693,#1141);
#913=LINE('',#6718,#1142);
#914=LINE('',#6743,#1143);
#915=LINE('',#6767,#1144);
#916=LINE('',#6792,#1145);
#917=LINE('',#6817,#1146);
#918=LINE('',#6841,#1147);
#919=LINE('',#6859,#1148);
#920=LINE('',#6866,#1149);
#921=LINE('',#9210,#1150);
#922=LINE('',#9212,#1151);
#923=LINE('',#9214,#1152);
#924=LINE('',#9215,#1153);
#925=LINE('',#9221,#1154);
#926=LINE('',#9224,#1155);
#927=LINE('',#9226,#1156);
#928=LINE('',#9227,#1157);
#929=LINE('',#9233,#1158);
#930=LINE('',#9236,#1159);
#931=LINE('',#9238,#1160);
#932=LINE('',#9239,#1161);
#933=LINE('',#9245,#1162);
#934=LINE('',#9248,#1163);
#935=LINE('',#9250,#1164);
#936=LINE('',#9251,#1165);
#937=LINE('',#9260,#1166);
#938=LINE('',#9263,#1167);
#939=LINE('',#9266,#1168);
#940=LINE('',#9268,#1169);
#941=LINE('',#9269,#1170);
#942=LINE('',#9275,#1171);
#943=LINE('',#9278,#1172);
#944=LINE('',#9280,#1173);
#945=LINE('',#9281,#1174);
#946=LINE('',#9284,#1175);
#947=LINE('',#9286,#1176);
#948=LINE('',#9287,#1177);
#949=LINE('',#9290,#1178);
#950=LINE('',#9292,#1179);
#951=LINE('',#9293,#1180);
#952=LINE('',#9296,#1181);
#953=LINE('',#9298,#1182);
#954=LINE('',#9299,#1183);
#955=LINE('',#9302,#1184);
#956=LINE('',#9304,#1185);
#957=LINE('',#9305,#1186);
#958=LINE('',#9311,#1187);
#959=LINE('',#9314,#1188);
#960=LINE('',#9316,#1189);
#961=LINE('',#9317,#1190);
#962=LINE('',#9323,#1191);
#963=LINE('',#9326,#1192);
#964=LINE('',#9328,#1193);
#965=LINE('',#9329,#1194);
#966=LINE('',#9332,#1195);
#967=LINE('',#9334,#1196);
#968=LINE('',#9335,#1197);
#969=LINE('',#9338,#1198);
#970=LINE('',#9340,#1199);
#971=LINE('',#9341,#1200);
#972=LINE('',#9344,#1201);
#973=LINE('',#9346,#1202);
#974=LINE('',#9347,#1203);
#975=LINE('',#9349,#1204);
#976=LINE('',#9350,#1205);
#977=LINE('',#9357,#1206);
#978=LINE('',#9359,#1207);
#979=LINE('',#9361,#1208);
#980=LINE('',#9362,#1209);
#981=LINE('',#9365,#1210);
#982=LINE('',#9367,#1211);
#983=LINE('',#9368,#1212);
#984=LINE('',#9371,#1213);
#985=LINE('',#9373,#1214);
#986=LINE('',#9374,#1215);
#987=LINE('',#9376,#1216);
#988=LINE('',#9377,#1217);
#989=LINE('',#9385,#1218);
#990=LINE('',#9391,#1219);
#991=LINE('',#9399,#1220);
#992=LINE('',#9423,#1221);
#993=LINE('',#9471,#1222);
#994=LINE('',#9519,#1223);
#995=LINE('',#9573,#1224);
#996=LINE('',#9621,#1225);
#997=LINE('',#9669,#1226);
#998=LINE('',#9717,#1227);
#999=LINE('',#9771,#1228);
#1000=LINE('',#9819,#1229);
#1001=LINE('',#9867,#1230);
#1002=LINE('',#9921,#1231);
#1003=LINE('',#9969,#1232);
#1004=LINE('',#10017,#1233);
#1005=LINE('',#10068,#1234);
#1006=LINE('',#10116,#1235);
#1007=LINE('',#10164,#1236);
#1008=LINE('',#10212,#1237);
#1009=LINE('',#10266,#1238);
#1010=LINE('',#10314,#1239);
#1011=LINE('',#10362,#1240);
#1012=LINE('',#10416,#1241);
#1013=LINE('',#10464,#1242);
#1014=LINE('',#10512,#1243);
#1015=LINE('',#10563,#1244);
#1016=LINE('',#10614,#1245);
#1017=LINE('',#10662,#1246);
#1018=LINE('',#10710,#1247);
#1019=LINE('',#10764,#1248);
#1020=LINE('',#10812,#1249);
#1021=LINE('',#10860,#1250);
#1022=LINE('',#10885,#1251);
#1023=LINE('',#10910,#1252);
#1024=LINE('',#10934,#1253);
#1025=LINE('',#10959,#1254);
#1026=LINE('',#10984,#1255);
#1027=LINE('',#11008,#1256);
#1028=LINE('',#11032,#1257);
#1029=LINE('',#11058,#1258);
#1030=LINE('',#11082,#1259);
#1031=LINE('',#11106,#1260);
#1032=LINE('',#11131,#1261);
#1033=LINE('',#11156,#1262);
#1034=LINE('',#11180,#1263);
#1035=LINE('',#11205,#1264);
#1036=LINE('',#11230,#1265);
#1037=LINE('',#11254,#1266);
#1038=LINE('',#11278,#1267);
#1039=LINE('',#11304,#1268);
#1040=LINE('',#11328,#1269);
#1041=LINE('',#11352,#1270);
#1042=LINE('',#11377,#1271);
#1043=LINE('',#11402,#1272);
#1044=LINE('',#11426,#1273);
#1045=LINE('',#11451,#1274);
#1046=LINE('',#11476,#1275);
#1047=LINE('',#11500,#1276);
#1048=LINE('',#11524,#1277);
#1049=LINE('',#11549,#1278);
#1050=LINE('',#11574,#1279);
#1051=LINE('',#11904,#1280);
#1052=LINE('',#13721,#1281);
#1053=LINE('',#13723,#1282);
#1054=LINE('',#13725,#1283);
#1055=LINE('',#13726,#1284);
#1056=LINE('',#13729,#1285);
#1057=LINE('',#13731,#1286);
#1058=LINE('',#13732,#1287);
#1059=LINE('',#13735,#1288);
#1060=LINE('',#13737,#1289);
#1061=LINE('',#13738,#1290);
#1062=LINE('',#13741,#1291);
#1063=LINE('',#13743,#1292);
#1064=LINE('',#13744,#1293);
#1065=LINE('',#13747,#1294);
#1066=LINE('',#13749,#1295);
#1067=LINE('',#13750,#1296);
#1068=LINE('',#13752,#1297);
#1069=LINE('',#13753,#1298);
#1070=LINE('',#13760,#1299);
#1071=LINE('',#13769,#1300);
#1072=VECTOR('',#4050,1.);
#1073=VECTOR('',#4059,1.);
#1074=VECTOR('',#4068,3.5);
#1075=VECTOR('',#4075,3.5);
#1076=VECTOR('',#4082,3.5);
#1077=VECTOR('',#4089,3.5);
#1078=VECTOR('',#4096,3.);
#1079=VECTOR('',#4103,3.);
#1080=VECTOR('',#4108,10.);
#1081=VECTOR('',#4109,10.);
#1082=VECTOR('',#4110,10.);
#1083=VECTOR('',#4111,10.);
#1084=VECTOR('',#4114,10.);
#1085=VECTOR('',#4115,10.);
#1086=VECTOR('',#4116,10.);
#1087=VECTOR('',#4119,10.);
#1088=VECTOR('',#4120,10.);
#1089=VECTOR('',#4121,10.);
#1090=VECTOR('',#4124,10.);
#1091=VECTOR('',#4125,10.);
#1092=VECTOR('',#4134,2.5);
#1093=VECTOR('',#4137,2.5);
#1094=VECTOR('',#4142,2.5);
#1095=VECTOR('',#4145,2.5);
#1096=VECTOR('',#4148,2.5);
#1097=VECTOR('',#4151,2.5);
#1098=VECTOR('',#4154,2.5);
#1099=VECTOR('',#4157,2.5);
#1100=VECTOR('',#4160,2.5);
#1101=VECTOR('',#4163,2.5);
#1102=VECTOR('',#4166,2.5);
#1103=VECTOR('',#4169,2.5);
#1104=VECTOR('',#4172,2.5);
#1105=VECTOR('',#4175,2.5);
#1106=VECTOR('',#4180,2.56);
#1107=VECTOR('',#4185,2.56);
#1108=VECTOR('',#4188,2.56);
#1109=VECTOR('',#4191,2.56);
#1110=VECTOR('',#4194,2.56);
#1111=VECTOR('',#4197,2.56);
#1112=VECTOR('',#4200,2.56);
#1113=VECTOR('',#4203,2.56);
#1114=VECTOR('',#4206,2.56);
#1115=VECTOR('',#4209,2.56);
#1116=VECTOR('',#4212,2.56);
#1117=VECTOR('',#4215,2.56);
#1118=VECTOR('',#4218,2.56);
#1119=VECTOR('',#4221,2.56);
#1120=VECTOR('',#4226,2.5);
#1121=VECTOR('',#4229,2.5);
#1122=VECTOR('',#4234,2.5);
#1123=VECTOR('',#4237,2.5);
#1124=VECTOR('',#4240,2.5);
#1125=VECTOR('',#4243,2.5);
#1126=VECTOR('',#4246,2.5);
#1127=VECTOR('',#4249,2.5);
#1128=VECTOR('',#4252,2.5);
#1129=VECTOR('',#4255,2.5);
#1130=VECTOR('',#4258,2.5);
#1131=VECTOR('',#4261,2.5);
#1132=VECTOR('',#4264,2.5);
#1133=VECTOR('',#4267,2.5);
#1134=VECTOR('',#4272,2.56);
#1135=VECTOR('',#4277,2.56);
#1136=VECTOR('',#4280,2.56);
#1137=VECTOR('',#4283,2.56);
#1138=VECTOR('',#4286,2.56);
#1139=VECTOR('',#4289,2.56);
#1140=VECTOR('',#4292,2.56);
#1141=VECTOR('',#4295,2.56);
#1142=VECTOR('',#4298,2.56);
#1143=VECTOR('',#4301,2.56);
#1144=VECTOR('',#4304,2.56);
#1145=VECTOR('',#4307,2.56);
#1146=VECTOR('',#4310,2.56);
#1147=VECTOR('',#4313,2.56);
#1148=VECTOR('',#4320,1.);
#1149=VECTOR('',#4329,1.);
#1150=VECTOR('',#4352,10.);
#1151=VECTOR('',#4353,10.);
#1152=VECTOR('',#4354,10.);
#1153=VECTOR('',#4355,10.);
#1154=VECTOR('',#4362,10.);
#1155=VECTOR('',#4365,10.);
#1156=VECTOR('',#4366,10.);
#1157=VECTOR('',#4367,10.);
#1158=VECTOR('',#4374,10.);
#1159=VECTOR('',#4377,10.);
#1160=VECTOR('',#4378,10.);
#1161=VECTOR('',#4379,10.);
#1162=VECTOR('',#4386,10.);
#1163=VECTOR('',#4389,10.);
#1164=VECTOR('',#4390,10.);
#1165=VECTOR('',#4391,10.);
#1166=VECTOR('',#4402,10.);
#1167=VECTOR('',#4405,10.);
#1168=VECTOR('',#4408,10.);
#1169=VECTOR('',#4409,10.);
#1170=VECTOR('',#4410,10.);
#1171=VECTOR('',#4417,10.);
#1172=VECTOR('',#4420,10.);
#1173=VECTOR('',#4421,10.);
#1174=VECTOR('',#4422,10.);
#1175=VECTOR('',#4425,10.);
#1176=VECTOR('',#4426,10.);
#1177=VECTOR('',#4427,10.);
#1178=VECTOR('',#4430,10.);
#1179=VECTOR('',#4431,10.);
#1180=VECTOR('',#4432,10.);
#1181=VECTOR('',#4435,10.);
#1182=VECTOR('',#4436,10.);
#1183=VECTOR('',#4437,10.);
#1184=VECTOR('',#4440,10.);
#1185=VECTOR('',#4441,10.);
#1186=VECTOR('',#4442,10.);
#1187=VECTOR('',#4449,10.);
#1188=VECTOR('',#4452,10.);
#1189=VECTOR('',#4453,10.);
#1190=VECTOR('',#4454,10.);
#1191=VECTOR('',#4461,10.);
#1192=VECTOR('',#4464,10.);
#1193=VECTOR('',#4465,10.);
#1194=VECTOR('',#4466,10.);
#1195=VECTOR('',#4469,10.);
#1196=VECTOR('',#4470,10.);
#1197=VECTOR('',#4471,10.);
#1198=VECTOR('',#4474,10.);
#1199=VECTOR('',#4475,10.);
#1200=VECTOR('',#4476,10.);
#1201=VECTOR('',#4479,10.);
#1202=VECTOR('',#4480,10.);
#1203=VECTOR('',#4481,10.);
#1204=VECTOR('',#4484,10.);
#1205=VECTOR('',#4485,10.);
#1206=VECTOR('',#4494,10.);
#1207=VECTOR('',#4495,10.);
#1208=VECTOR('',#4496,10.);
#1209=VECTOR('',#4497,10.);
#1210=VECTOR('',#4500,10.);
#1211=VECTOR('',#4501,10.);
#1212=VECTOR('',#4502,10.);
#1213=VECTOR('',#4505,10.);
#1214=VECTOR('',#4506,10.);
#1215=VECTOR('',#4507,10.);
#1216=VECTOR('',#4510,10.);
#1217=VECTOR('',#4511,10.);
#1218=VECTOR('',#4522,3.);
#1219=VECTOR('',#4529,6.);
#1220=VECTOR('',#4540,2.5);
#1221=VECTOR('',#4545,2.5);
#1222=VECTOR('',#4548,2.5);
#1223=VECTOR('',#4551,2.5);
#1224=VECTOR('',#4554,2.5);
#1225=VECTOR('',#4557,2.5);
#1226=VECTOR('',#4560,2.5);
#1227=VECTOR('',#4563,2.5);
#1228=VECTOR('',#4566,2.5);
#1229=VECTOR('',#4569,2.5);
#1230=VECTOR('',#4572,2.5);
#1231=VECTOR('',#4575,2.5);
#1232=VECTOR('',#4578,2.5);
#1233=VECTOR('',#4581,2.5);
#1234=VECTOR('',#4584,2.5);
#1235=VECTOR('',#4587,2.5);
#1236=VECTOR('',#4590,2.5);
#1237=VECTOR('',#4593,2.5);
#1238=VECTOR('',#4596,2.5);
#1239=VECTOR('',#4599,2.5);
#1240=VECTOR('',#4602,2.5);
#1241=VECTOR('',#4605,2.5);
#1242=VECTOR('',#4608,2.5);
#1243=VECTOR('',#4611,2.5);
#1244=VECTOR('',#4614,2.5);
#1245=VECTOR('',#4617,2.5);
#1246=VECTOR('',#4620,2.5);
#1247=VECTOR('',#4623,2.5);
#1248=VECTOR('',#4626,2.5);
#1249=VECTOR('',#4629,2.5);
#1250=VECTOR('',#4632,1.99475);
#1251=VECTOR('',#4637,1.99475);
#1252=VECTOR('',#4640,1.99475);
#1253=VECTOR('',#4643,1.99475);
#1254=VECTOR('',#4646,1.99475);
#1255=VECTOR('',#4649,1.99475);
#1256=VECTOR('',#4652,1.99475);
#1257=VECTOR('',#4655,1.99475);
#1258=VECTOR('',#4658,1.99475);
#1259=VECTOR('',#4661,1.99475);
#1260=VECTOR('',#4664,1.99475);
#1261=VECTOR('',#4667,1.99475);
#1262=VECTOR('',#4670,1.99475);
#1263=VECTOR('',#4673,1.99475);
#1264=VECTOR('',#4676,1.99475);
#1265=VECTOR('',#4679,1.99475);
#1266=VECTOR('',#4682,1.99475);
#1267=VECTOR('',#4685,1.99475);
#1268=VECTOR('',#4688,1.99475);
#1269=VECTOR('',#4691,1.99475);
#1270=VECTOR('',#4694,1.99475);
#1271=VECTOR('',#4697,1.99475);
#1272=VECTOR('',#4700,1.99475);
#1273=VECTOR('',#4703,1.99475);
#1274=VECTOR('',#4706,1.99475);
#1275=VECTOR('',#4709,1.99475);
#1276=VECTOR('',#4712,1.99475);
#1277=VECTOR('',#4715,1.99475);
#1278=VECTOR('',#4718,1.99475);
#1279=VECTOR('',#4721,1.99475);
#1280=VECTOR('',#4726,2.);
#1281=VECTOR('',#4737,10.);
#1282=VECTOR('',#4738,10.);
#1283=VECTOR('',#4739,10.);
#1284=VECTOR('',#4740,10.);
#1285=VECTOR('',#4743,10.);
#1286=VECTOR('',#4744,10.);
#1287=VECTOR('',#4745,10.);
#1288=VECTOR('',#4748,10.);
#1289=VECTOR('',#4749,10.);
#1290=VECTOR('',#4750,10.);
#1291=VECTOR('',#4753,10.);
#1292=VECTOR('',#4754,10.);
#1293=VECTOR('',#4755,10.);
#1294=VECTOR('',#4758,10.);
#1295=VECTOR('',#4759,10.);
#1296=VECTOR('',#4760,10.);
#1297=VECTOR('',#4763,10.);
#1298=VECTOR('',#4764,10.);
#1299=VECTOR('',#4773,4.);
#1300=VECTOR('',#4786,1.);
#1301=CIRCLE('',#3771,1.);
#1302=CIRCLE('',#3772,1.);
#1303=CIRCLE('',#3775,1.);
#1304=CIRCLE('',#3776,1.);
#1305=CIRCLE('',#3779,3.5);
#1306=CIRCLE('',#3780,3.5);
#1307=CIRCLE('',#3782,3.5);
#1308=CIRCLE('',#3783,3.5);
#1309=CIRCLE('',#3785,3.5);
#1310=CIRCLE('',#3786,3.5);
#1311=CIRCLE('',#3788,3.5);
#1312=CIRCLE('',#3789,3.5);
#1313=CIRCLE('',#3791,3.);
#1314=CIRCLE('',#3792,3.);
#1315=CIRCLE('',#3794,3.);
#1316=CIRCLE('',#3795,3.);
#1317=CIRCLE('',#3804,2.117);
#1318=CIRCLE('',#3805,2.117);
#1319=CIRCLE('',#3818,2.117);
#1320=CIRCLE('',#3820,2.56);
#1321=CIRCLE('',#3834,2.56);
#1322=CIRCLE('',#3836,2.117);
#1323=CIRCLE('',#3837,2.117);
#1324=CIRCLE('',#3850,2.117);
#1325=CIRCLE('',#3852,2.56);
#1326=CIRCLE('',#3866,2.56);
#1327=CIRCLE('',#3868,1.);
#1328=CIRCLE('',#3869,1.);
#1329=CIRCLE('',#3872,1.);
#1330=CIRCLE('',#3873,1.);
#1331=CIRCLE('',#3885,1.99999999999999);
#1332=CIRCLE('',#3886,1.99999999999999);
#1333=CIRCLE('',#3889,1.99999999999999);
#1334=CIRCLE('',#3890,1.99999999999999);
#1335=CIRCLE('',#3893,2.);
#1336=CIRCLE('',#3894,2.);
#1337=CIRCLE('',#3897,2.);
#1338=CIRCLE('',#3898,2.);
#1339=CIRCLE('',#3900,2.);
#1340=CIRCLE('',#3901,2.);
#1341=CIRCLE('',#3904,2.00000000000001);
#1342=CIRCLE('',#3905,2.00000000000001);
#1343=CIRCLE('',#3912,2.00000000000001);
#1344=CIRCLE('',#3913,2.00000000000001);
#1345=CIRCLE('',#3916,2.);
#1346=CIRCLE('',#3917,2.);
#1347=CIRCLE('',#3934,3.);
#1348=CIRCLE('',#3935,3.);
#1349=CIRCLE('',#3937,6.);
#1350=CIRCLE('',#3938,6.);
#1351=CIRCLE('',#3943,2.4505);
#1352=CIRCLE('',#3974,1.99475);
#1353=CIRCLE('',#4005,2.4505);
#1354=CIRCLE('',#4006,1.5);
#1355=CIRCLE('',#4008,1.99475);
#1356=CIRCLE('',#4018,4.);
#1357=CIRCLE('',#4020,4.);
#1358=CIRCLE('',#4025,1.);
#1359=CIRCLE('',#4026,1.);
#1360=VERTEX_POINT('',#4819);
#1361=VERTEX_POINT('',#4821);
#1362=VERTEX_POINT('',#4826);
#1363=VERTEX_POINT('',#4828);
#1364=VERTEX_POINT('',#4833);
#1365=VERTEX_POINT('',#4835);
#1366=VERTEX_POINT('',#4839);
#1367=VERTEX_POINT('',#4841);
#1368=VERTEX_POINT('',#4845);
#1369=VERTEX_POINT('',#4847);
#1370=VERTEX_POINT('',#4851);
#1371=VERTEX_POINT('',#4853);
#1372=VERTEX_POINT('',#4857);
#1373=VERTEX_POINT('',#4859);
#1374=VERTEX_POINT('',#4863);
#1375=VERTEX_POINT('',#4865);
#1376=VERTEX_POINT('',#4869);
#1377=VERTEX_POINT('',#4870);
#1378=VERTEX_POINT('',#4872);
#1379=VERTEX_POINT('',#4874);
#1380=VERTEX_POINT('',#4878);
#1381=VERTEX_POINT('',#4880);
#1382=VERTEX_POINT('',#4884);
#1383=VERTEX_POINT('',#4886);
#1384=VERTEX_POINT('',#4896);
#1385=VERTEX_POINT('',#4897);
#1386=VERTEX_POINT('',#4899);
#1387=VERTEX_POINT('',#4919);
#1388=VERTEX_POINT('',#4921);
#1389=VERTEX_POINT('',#4926);
#1390=VERTEX_POINT('',#4955);
#1391=VERTEX_POINT('',#4956);
#1392=VERTEX_POINT('',#5003);
#1393=VERTEX_POINT('',#5004);
#1394=VERTEX_POINT('',#5054);
#1395=VERTEX_POINT('',#5055);
#1396=VERTEX_POINT('',#5105);
#1397=VERTEX_POINT('',#5106);
#1398=VERTEX_POINT('',#5153);
#1399=VERTEX_POINT('',#5154);
#1400=VERTEX_POINT('',#5204);
#1401=VERTEX_POINT('',#5205);
#1402=VERTEX_POINT('',#5255);
#1403=VERTEX_POINT('',#5256);
#1404=VERTEX_POINT('',#5303);
#1405=VERTEX_POINT('',#5304);
#1406=VERTEX_POINT('',#5354);
#1407=VERTEX_POINT('',#5355);
#1408=VERTEX_POINT('',#5405);
#1409=VERTEX_POINT('',#5406);
#1410=VERTEX_POINT('',#5453);
#1411=VERTEX_POINT('',#5454);
#1412=VERTEX_POINT('',#5504);
#1413=VERTEX_POINT('',#5505);
#1414=VERTEX_POINT('',#5507);
#1415=VERTEX_POINT('',#5521);
#1416=VERTEX_POINT('',#5543);
#1417=VERTEX_POINT('',#5544);
#1418=VERTEX_POINT('',#5546);
#1419=VERTEX_POINT('',#5553);
#1420=VERTEX_POINT('',#5563);
#1421=VERTEX_POINT('',#5564);
#1422=VERTEX_POINT('',#5588);
#1423=VERTEX_POINT('',#5589);
#1424=VERTEX_POINT('',#5613);
#1425=VERTEX_POINT('',#5614);
#1426=VERTEX_POINT('',#5637);
#1427=VERTEX_POINT('',#5638);
#1428=VERTEX_POINT('',#5662);
#1429=VERTEX_POINT('',#5663);
#1430=VERTEX_POINT('',#5687);
#1431=VERTEX_POINT('',#5688);
#1432=VERTEX_POINT('',#5711);
#1433=VERTEX_POINT('',#5712);
#1434=VERTEX_POINT('',#5736);
#1435=VERTEX_POINT('',#5737);
#1436=VERTEX_POINT('',#5761);
#1437=VERTEX_POINT('',#5762);
#1438=VERTEX_POINT('',#5785);
#1439=VERTEX_POINT('',#5786);
#1440=VERTEX_POINT('',#5810);
#1441=VERTEX_POINT('',#5811);
#1442=VERTEX_POINT('',#5835);
#1443=VERTEX_POINT('',#5836);
#1444=VERTEX_POINT('',#5859);
#1445=VERTEX_POINT('',#5860);
#1446=VERTEX_POINT('',#5862);
#1447=VERTEX_POINT('',#5868);
#1448=VERTEX_POINT('',#5876);
#1449=VERTEX_POINT('',#5877);
#1450=VERTEX_POINT('',#5879);
#1451=VERTEX_POINT('',#5899);
#1452=VERTEX_POINT('',#5901);
#1453=VERTEX_POINT('',#5906);
#1454=VERTEX_POINT('',#5935);
#1455=VERTEX_POINT('',#5936);
#1456=VERTEX_POINT('',#5983);
#1457=VERTEX_POINT('',#5984);
#1458=VERTEX_POINT('',#6034);
#1459=VERTEX_POINT('',#6035);
#1460=VERTEX_POINT('',#6085);
#1461=VERTEX_POINT('',#6086);
#1462=VERTEX_POINT('',#6133);
#1463=VERTEX_POINT('',#6134);
#1464=VERTEX_POINT('',#6184);
#1465=VERTEX_POINT('',#6185);
#1466=VERTEX_POINT('',#6235);
#1467=VERTEX_POINT('',#6236);
#1468=VERTEX_POINT('',#6283);
#1469=VERTEX_POINT('',#6284);
#1470=VERTEX_POINT('',#6334);
#1471=VERTEX_POINT('',#6335);
#1472=VERTEX_POINT('',#6385);
#1473=VERTEX_POINT('',#6386);
#1474=VERTEX_POINT('',#6433);
#1475=VERTEX_POINT('',#6434);
#1476=VERTEX_POINT('',#6484);
#1477=VERTEX_POINT('',#6485);
#1478=VERTEX_POINT('',#6487);
#1479=VERTEX_POINT('',#6501);
#1480=VERTEX_POINT('',#6523);
#1481=VERTEX_POINT('',#6524);
#1482=VERTEX_POINT('',#6526);
#1483=VERTEX_POINT('',#6533);
#1484=VERTEX_POINT('',#6543);
#1485=VERTEX_POINT('',#6544);
#1486=VERTEX_POINT('',#6568);
#1487=VERTEX_POINT('',#6569);
#1488=VERTEX_POINT('',#6593);
#1489=VERTEX_POINT('',#6594);
#1490=VERTEX_POINT('',#6617);
#1491=VERTEX_POINT('',#6618);
#1492=VERTEX_POINT('',#6642);
#1493=VERTEX_POINT('',#6643);
#1494=VERTEX_POINT('',#6667);
#1495=VERTEX_POINT('',#6668);
#1496=VERTEX_POINT('',#6691);
#1497=VERTEX_POINT('',#6692);
#1498=VERTEX_POINT('',#6716);
#1499=VERTEX_POINT('',#6717);
#1500=VERTEX_POINT('',#6741);
#1501=VERTEX_POINT('',#6742);
#1502=VERTEX_POINT('',#6765);
#1503=VERTEX_POINT('',#6766);
#1504=VERTEX_POINT('',#6790);
#1505=VERTEX_POINT('',#6791);
#1506=VERTEX_POINT('',#6815);
#1507=VERTEX_POINT('',#6816);
#1508=VERTEX_POINT('',#6839);
#1509=VERTEX_POINT('',#6840);
#1510=VERTEX_POINT('',#6842);
#1511=VERTEX_POINT('',#6848);
#1512=VERTEX_POINT('',#6856);
#1513=VERTEX_POINT('',#6858);
#1514=VERTEX_POINT('',#6863);
#1515=VERTEX_POINT('',#6865);
#1516=VERTEX_POINT('',#9208);
#1517=VERTEX_POINT('',#9209);
#1518=VERTEX_POINT('',#9211);
#1519=VERTEX_POINT('',#9213);
#1520=VERTEX_POINT('',#9217);
#1521=VERTEX_POINT('',#9219);
#1522=VERTEX_POINT('',#9223);
#1523=VERTEX_POINT('',#9225);
#1524=VERTEX_POINT('',#9229);
#1525=VERTEX_POINT('',#9231);
#1526=VERTEX_POINT('',#9235);
#1527=VERTEX_POINT('',#9237);
#1528=VERTEX_POINT('',#9241);
#1529=VERTEX_POINT('',#9243);
#1530=VERTEX_POINT('',#9247);
#1531=VERTEX_POINT('',#9249);
#1532=VERTEX_POINT('',#9256);
#1533=VERTEX_POINT('',#9257);
#1534=VERTEX_POINT('',#9259);
#1535=VERTEX_POINT('',#9261);
#1536=VERTEX_POINT('',#9265);
#1537=VERTEX_POINT('',#9267);
#1538=VERTEX_POINT('',#9271);
#1539=VERTEX_POINT('',#9273);
#1540=VERTEX_POINT('',#9277);
#1541=VERTEX_POINT('',#9279);
#1542=VERTEX_POINT('',#9283);
#1543=VERTEX_POINT('',#9285);
#1544=VERTEX_POINT('',#9289);
#1545=VERTEX_POINT('',#9291);
#1546=VERTEX_POINT('',#9295);
#1547=VERTEX_POINT('',#9297);
#1548=VERTEX_POINT('',#9301);
#1549=VERTEX_POINT('',#9303);
#1550=VERTEX_POINT('',#9307);
#1551=VERTEX_POINT('',#9309);
#1552=VERTEX_POINT('',#9313);
#1553=VERTEX_POINT('',#9315);
#1554=VERTEX_POINT('',#9319);
#1555=VERTEX_POINT('',#9321);
#1556=VERTEX_POINT('',#9325);
#1557=VERTEX_POINT('',#9327);
#1558=VERTEX_POINT('',#9331);
#1559=VERTEX_POINT('',#9333);
#1560=VERTEX_POINT('',#9337);
#1561=VERTEX_POINT('',#9339);
#1562=VERTEX_POINT('',#9343);
#1563=VERTEX_POINT('',#9345);
#1564=VERTEX_POINT('',#9355);
#1565=VERTEX_POINT('',#9356);
#1566=VERTEX_POINT('',#9358);
#1567=VERTEX_POINT('',#9360);
#1568=VERTEX_POINT('',#9364);
#1569=VERTEX_POINT('',#9366);
#1570=VERTEX_POINT('',#9370);
#1571=VERTEX_POINT('',#9372);
#1572=VERTEX_POINT('',#9382);
#1573=VERTEX_POINT('',#9384);
#1574=VERTEX_POINT('',#9388);
#1575=VERTEX_POINT('',#9390);
#1576=VERTEX_POINT('',#9397);
#1577=VERTEX_POINT('',#9398);
#1578=VERTEX_POINT('',#9400);
#1579=VERTEX_POINT('',#9411);
#1580=VERTEX_POINT('',#9421);
#1581=VERTEX_POINT('',#9422);
#1582=VERTEX_POINT('',#9469);
#1583=VERTEX_POINT('',#9470);
#1584=VERTEX_POINT('',#9517);
#1585=VERTEX_POINT('',#9518);
#1586=VERTEX_POINT('',#9571);
#1587=VERTEX_POINT('',#9572);
#1588=VERTEX_POINT('',#9619);
#1589=VERTEX_POINT('',#9620);
#1590=VERTEX_POINT('',#9667);
#1591=VERTEX_POINT('',#9668);
#1592=VERTEX_POINT('',#9715);
#1593=VERTEX_POINT('',#9716);
#1594=VERTEX_POINT('',#9769);
#1595=VERTEX_POINT('',#9770);
#1596=VERTEX_POINT('',#9817);
#1597=VERTEX_POINT('',#9818);
#1598=VERTEX_POINT('',#9865);
#1599=VERTEX_POINT('',#9866);
#1600=VERTEX_POINT('',#9919);
#1601=VERTEX_POINT('',#9920);
#1602=VERTEX_POINT('',#9967);
#1603=VERTEX_POINT('',#9968);
#1604=VERTEX_POINT('',#10015);
#1605=VERTEX_POINT('',#10016);
#1606=VERTEX_POINT('',#10066);
#1607=VERTEX_POINT('',#10067);
#1608=VERTEX_POINT('',#10114);
#1609=VERTEX_POINT('',#10115);
#1610=VERTEX_POINT('',#10162);
#1611=VERTEX_POINT('',#10163);
#1612=VERTEX_POINT('',#10210);
#1613=VERTEX_POINT('',#10211);
#1614=VERTEX_POINT('',#10264);
#1615=VERTEX_POINT('',#10265);
#1616=VERTEX_POINT('',#10312);
#1617=VERTEX_POINT('',#10313);
#1618=VERTEX_POINT('',#10360);
#1619=VERTEX_POINT('',#10361);
#1620=VERTEX_POINT('',#10414);
#1621=VERTEX_POINT('',#10415);
#1622=VERTEX_POINT('',#10462);
#1623=VERTEX_POINT('',#10463);
#1624=VERTEX_POINT('',#10510);
#1625=VERTEX_POINT('',#10511);
#1626=VERTEX_POINT('',#10561);
#1627=VERTEX_POINT('',#10562);
#1628=VERTEX_POINT('',#10612);
#1629=VERTEX_POINT('',#10613);
#1630=VERTEX_POINT('',#10660);
#1631=VERTEX_POINT('',#10661);
#1632=VERTEX_POINT('',#10708);
#1633=VERTEX_POINT('',#10709);
#1634=VERTEX_POINT('',#10762);
#1635=VERTEX_POINT('',#10763);
#1636=VERTEX_POINT('',#10810);
#1637=VERTEX_POINT('',#10811);
#1638=VERTEX_POINT('',#10858);
#1639=VERTEX_POINT('',#10859);
#1640=VERTEX_POINT('',#10861);
#1641=VERTEX_POINT('',#10872);
#1642=VERTEX_POINT('',#10883);
#1643=VERTEX_POINT('',#10884);
#1644=VERTEX_POINT('',#10908);
#1645=VERTEX_POINT('',#10909);
#1646=VERTEX_POINT('',#10932);
#1647=VERTEX_POINT('',#10933);
#1648=VERTEX_POINT('',#10957);
#1649=VERTEX_POINT('',#10958);
#1650=VERTEX_POINT('',#10982);
#1651=VERTEX_POINT('',#10983);
#1652=VERTEX_POINT('',#11006);
#1653=VERTEX_POINT('',#11007);
#1654=VERTEX_POINT('',#11030);
#1655=VERTEX_POINT('',#11031);
#1656=VERTEX_POINT('',#11056);
#1657=VERTEX_POINT('',#11057);
#1658=VERTEX_POINT('',#11080);
#1659=VERTEX_POINT('',#11081);
#1660=VERTEX_POINT('',#11104);
#1661=VERTEX_POINT('',#11105);
#1662=VERTEX_POINT('',#11129);
#1663=VERTEX_POINT('',#11130);
#1664=VERTEX_POINT('',#11154);
#1665=VERTEX_POINT('',#11155);
#1666=VERTEX_POINT('',#11178);
#1667=VERTEX_POINT('',#11179);
#1668=VERTEX_POINT('',#11203);
#1669=VERTEX_POINT('',#11204);
#1670=VERTEX_POINT('',#11228);
#1671=VERTEX_POINT('',#11229);
#1672=VERTEX_POINT('',#11252);
#1673=VERTEX_POINT('',#11253);
#1674=VERTEX_POINT('',#11276);
#1675=VERTEX_POINT('',#11277);
#1676=VERTEX_POINT('',#11302);
#1677=VERTEX_POINT('',#11303);
#1678=VERTEX_POINT('',#11326);
#1679=VERTEX_POINT('',#11327);
#1680=VERTEX_POINT('',#11350);
#1681=VERTEX_POINT('',#11351);
#1682=VERTEX_POINT('',#11375);
#1683=VERTEX_POINT('',#11376);
#1684=VERTEX_POINT('',#11400);
#1685=VERTEX_POINT('',#11401);
#1686=VERTEX_POINT('',#11424);
#1687=VERTEX_POINT('',#11425);
#1688=VERTEX_POINT('',#11449);
#1689=VERTEX_POINT('',#11450);
#1690=VERTEX_POINT('',#11474);
#1691=VERTEX_POINT('',#11475);
#1692=VERTEX_POINT('',#11498);
#1693=VERTEX_POINT('',#11499);
#1694=VERTEX_POINT('',#11522);
#1695=VERTEX_POINT('',#11523);
#1696=VERTEX_POINT('',#11547);
#1697=VERTEX_POINT('',#11548);
#1698=VERTEX_POINT('',#11572);
#1699=VERTEX_POINT('',#11573);
#1700=VERTEX_POINT('',#11596);
#1701=VERTEX_POINT('',#11811);
#1702=VERTEX_POINT('',#11873);
#1703=VERTEX_POINT('',#11903);
#1704=VERTEX_POINT('',#12690);
#1705=VERTEX_POINT('',#12807);
#1706=VERTEX_POINT('',#13719);
#1707=VERTEX_POINT('',#13720);
#1708=VERTEX_POINT('',#13722);
#1709=VERTEX_POINT('',#13724);
#1710=VERTEX_POINT('',#13728);
#1711=VERTEX_POINT('',#13730);
#1712=VERTEX_POINT('',#13734);
#1713=VERTEX_POINT('',#13736);
#1714=VERTEX_POINT('',#13740);
#1715=VERTEX_POINT('',#13742);
#1716=VERTEX_POINT('',#13746);
#1717=VERTEX_POINT('',#13748);
#1718=VERTEX_POINT('',#13756);
#1719=VERTEX_POINT('',#13759);
#1720=VERTEX_POINT('',#13766);
#1721=VERTEX_POINT('',#13768);
#1722=EDGE_CURVE('',#1360,#1360,#1301,.T.);
#1723=EDGE_CURVE('',#1360,#1361,#843,.T.);
#1724=EDGE_CURVE('',#1361,#1361,#1302,.T.);
#1725=EDGE_CURVE('',#1362,#1362,#1303,.T.);
#1726=EDGE_CURVE('',#1362,#1363,#844,.T.);
#1727=EDGE_CURVE('',#1363,#1363,#1304,.T.);
#1728=EDGE_CURVE('',#1364,#1364,#1305,.T.);
#1729=EDGE_CURVE('',#1364,#1365,#845,.T.);
#1730=EDGE_CURVE('',#1365,#1365,#1306,.T.);
#1731=EDGE_CURVE('',#1366,#1366,#1307,.T.);
#1732=EDGE_CURVE('',#1366,#1367,#846,.T.);
#1733=EDGE_CURVE('',#1367,#1367,#1308,.T.);
#1734=EDGE_CURVE('',#1368,#1368,#1309,.T.);
#1735=EDGE_CURVE('',#1368,#1369,#847,.T.);
#1736=EDGE_CURVE('',#1369,#1369,#1310,.T.);
#1737=EDGE_CURVE('',#1370,#1370,#1311,.T.);
#1738=EDGE_CURVE('',#1370,#1371,#848,.T.);
#1739=EDGE_CURVE('',#1371,#1371,#1312,.T.);
#1740=EDGE_CURVE('',#1372,#1372,#1313,.T.);
#1741=EDGE_CURVE('',#1372,#1373,#849,.T.);
#1742=EDGE_CURVE('',#1373,#1373,#1314,.T.);
#1743=EDGE_CURVE('',#1374,#1374,#1315,.T.);
#1744=EDGE_CURVE('',#1374,#1375,#850,.T.);
#1745=EDGE_CURVE('',#1375,#1375,#1316,.T.);
#1746=EDGE_CURVE('',#1376,#1377,#851,.T.);
#1747=EDGE_CURVE('',#1377,#1378,#852,.T.);
#1748=EDGE_CURVE('',#1379,#1378,#853,.T.);
#1749=EDGE_CURVE('',#1376,#1379,#854,.T.);
#1750=EDGE_CURVE('',#1380,#1376,#855,.T.);
#1751=EDGE_CURVE('',#1381,#1379,#856,.T.);
#1752=EDGE_CURVE('',#1380,#1381,#857,.T.);
#1753=EDGE_CURVE('',#1382,#1380,#858,.T.);
#1754=EDGE_CURVE('',#1383,#1381,#859,.T.);
#1755=EDGE_CURVE('',#1382,#1383,#860,.T.);
#1756=EDGE_CURVE('',#1377,#1382,#861,.T.);
#1757=EDGE_CURVE('',#1378,#1383,#862,.T.);
#1758=EDGE_CURVE('',#1384,#1385,#863,.T.);
#1759=EDGE_CURVE('',#1385,#1386,#62,.T.);
#1760=EDGE_CURVE('',#1386,#1387,#1317,.T.);
#1761=EDGE_CURVE('',#1387,#1388,#63,.T.);
#1762=EDGE_CURVE('',#1388,#1389,#864,.T.);
#1763=EDGE_CURVE('',#1389,#1389,#1318,.F.);
#1764=EDGE_CURVE('',#1388,#1384,#64,.T.);
#1765=EDGE_CURVE('',#1390,#1391,#865,.T.);
#1766=EDGE_CURVE('',#1391,#1385,#65,.T.);
#1767=EDGE_CURVE('',#1384,#1390,#66,.T.);
#1768=EDGE_CURVE('',#1392,#1393,#866,.T.);
#1769=EDGE_CURVE('',#1393,#1391,#67,.T.);
#1770=EDGE_CURVE('',#1390,#1392,#68,.T.);
#1771=EDGE_CURVE('',#1394,#1395,#867,.T.);
#1772=EDGE_CURVE('',#1395,#1393,#69,.T.);
#1773=EDGE_CURVE('',#1392,#1394,#70,.T.);
#1774=EDGE_CURVE('',#1396,#1397,#868,.T.);
#1775=EDGE_CURVE('',#1397,#1395,#71,.T.);
#1776=EDGE_CURVE('',#1394,#1396,#72,.T.);
#1777=EDGE_CURVE('',#1398,#1399,#869,.T.);
#1778=EDGE_CURVE('',#1399,#1397,#73,.T.);
#1779=EDGE_CURVE('',#1396,#1398,#74,.T.);
#1780=EDGE_CURVE('',#1400,#1401,#870,.T.);
#1781=EDGE_CURVE('',#1401,#1399,#75,.T.);
#1782=EDGE_CURVE('',#1398,#1400,#76,.T.);
#1783=EDGE_CURVE('',#1402,#1403,#871,.T.);
#1784=EDGE_CURVE('',#1403,#1401,#77,.T.);
#1785=EDGE_CURVE('',#1400,#1402,#78,.T.);
#1786=EDGE_CURVE('',#1404,#1405,#872,.T.);
#1787=EDGE_CURVE('',#1405,#1403,#79,.T.);
#1788=EDGE_CURVE('',#1402,#1404,#80,.T.);
#1789=EDGE_CURVE('',#1406,#1407,#873,.T.);
#1790=EDGE_CURVE('',#1407,#1405,#81,.T.);
#1791=EDGE_CURVE('',#1404,#1406,#82,.T.);
#1792=EDGE_CURVE('',#1408,#1409,#874,.T.);
#1793=EDGE_CURVE('',#1409,#1407,#83,.T.);
#1794=EDGE_CURVE('',#1406,#1408,#84,.T.);
#1795=EDGE_CURVE('',#1410,#1411,#875,.T.);
#1796=EDGE_CURVE('',#1411,#1409,#85,.T.);
#1797=EDGE_CURVE('',#1408,#1410,#86,.T.);
#1798=EDGE_CURVE('',#1412,#1413,#876,.T.);
#1799=EDGE_CURVE('',#1412,#1414,#87,.T.);
#1800=EDGE_CURVE('',#1415,#1414,#1319,.T.);
#1801=EDGE_CURVE('',#1415,#1413,#88,.T.);
#1802=EDGE_CURVE('',#1416,#1417,#877,.T.);
#1803=EDGE_CURVE('',#1417,#1418,#89,.T.);
#1804=EDGE_CURVE('',#1419,#1418,#1320,.T.);
#1805=EDGE_CURVE('',#1416,#1419,#90,.T.);
#1806=EDGE_CURVE('',#1420,#1421,#878,.T.);
#1807=EDGE_CURVE('',#1421,#1417,#91,.T.);
#1808=EDGE_CURVE('',#1420,#1416,#92,.T.);
#1809=EDGE_CURVE('',#1422,#1423,#879,.T.);
#1810=EDGE_CURVE('',#1423,#1421,#93,.T.);
#1811=EDGE_CURVE('',#1422,#1420,#94,.T.);
#1812=EDGE_CURVE('',#1424,#1425,#880,.T.);
#1813=EDGE_CURVE('',#1425,#1423,#95,.T.);
#1814=EDGE_CURVE('',#1424,#1422,#96,.T.);
#1815=EDGE_CURVE('',#1426,#1427,#881,.T.);
#1816=EDGE_CURVE('',#1427,#1425,#97,.T.);
#1817=EDGE_CURVE('',#1426,#1424,#98,.T.);
#1818=EDGE_CURVE('',#1428,#1429,#882,.T.);
#1819=EDGE_CURVE('',#1429,#1427,#99,.T.);
#1820=EDGE_CURVE('',#1428,#1426,#100,.T.);
#1821=EDGE_CURVE('',#1430,#1431,#883,.T.);
#1822=EDGE_CURVE('',#1431,#1429,#101,.T.);
#1823=EDGE_CURVE('',#1430,#1428,#102,.T.);
#1824=EDGE_CURVE('',#1432,#1433,#884,.T.);
#1825=EDGE_CURVE('',#1433,#1431,#103,.T.);
#1826=EDGE_CURVE('',#1432,#1430,#104,.T.);
#1827=EDGE_CURVE('',#1434,#1435,#885,.T.);
#1828=EDGE_CURVE('',#1435,#1433,#105,.T.);
#1829=EDGE_CURVE('',#1434,#1432,#106,.T.);
#1830=EDGE_CURVE('',#1436,#1437,#886,.T.);
#1831=EDGE_CURVE('',#1437,#1435,#107,.T.);
#1832=EDGE_CURVE('',#1436,#1434,#108,.T.);
#1833=EDGE_CURVE('',#1438,#1439,#887,.T.);
#1834=EDGE_CURVE('',#1439,#1437,#109,.T.);
#1835=EDGE_CURVE('',#1438,#1436,#110,.T.);
#1836=EDGE_CURVE('',#1440,#1441,#888,.T.);
#1837=EDGE_CURVE('',#1441,#1439,#111,.T.);
#1838=EDGE_CURVE('',#1440,#1438,#112,.T.);
#1839=EDGE_CURVE('',#1442,#1443,#889,.T.);
#1840=EDGE_CURVE('',#1443,#1441,#113,.T.);
#1841=EDGE_CURVE('',#1442,#1440,#114,.T.);
#1842=EDGE_CURVE('',#1444,#1445,#890,.T.);
#1843=EDGE_CURVE('',#1446,#1444,#115,.T.);
#1844=EDGE_CURVE('',#1447,#1446,#1321,.T.);
#1845=EDGE_CURVE('',#1447,#1445,#116,.T.);
#1846=EDGE_CURVE('',#1448,#1449,#891,.T.);
#1847=EDGE_CURVE('',#1449,#1450,#117,.T.);
#1848=EDGE_CURVE('',#1450,#1451,#1322,.T.);
#1849=EDGE_CURVE('',#1451,#1452,#118,.T.);
#1850=EDGE_CURVE('',#1452,#1453,#892,.T.);
#1851=EDGE_CURVE('',#1453,#1453,#1323,.F.);
#1852=EDGE_CURVE('',#1452,#1448,#119,.T.);
#1853=EDGE_CURVE('',#1454,#1455,#893,.T.);
#1854=EDGE_CURVE('',#1455,#1449,#120,.T.);
#1855=EDGE_CURVE('',#1448,#1454,#121,.T.);
#1856=EDGE_CURVE('',#1456,#1457,#894,.T.);
#1857=EDGE_CURVE('',#1457,#1455,#122,.T.);
#1858=EDGE_CURVE('',#1454,#1456,#123,.T.);
#1859=EDGE_CURVE('',#1458,#1459,#895,.T.);
#1860=EDGE_CURVE('',#1459,#1457,#124,.T.);
#1861=EDGE_CURVE('',#1456,#1458,#125,.T.);
#1862=EDGE_CURVE('',#1460,#1461,#896,.T.);
#1863=EDGE_CURVE('',#1461,#1459,#126,.T.);
#1864=EDGE_CURVE('',#1458,#1460,#127,.T.);
#1865=EDGE_CURVE('',#1462,#1463,#897,.T.);
#1866=EDGE_CURVE('',#1463,#1461,#128,.T.);
#1867=EDGE_CURVE('',#1460,#1462,#129,.T.);
#1868=EDGE_CURVE('',#1464,#1465,#898,.T.);
#1869=EDGE_CURVE('',#1465,#1463,#130,.T.);
#1870=EDGE_CURVE('',#1462,#1464,#131,.T.);
#1871=EDGE_CURVE('',#1466,#1467,#899,.T.);
#1872=EDGE_CURVE('',#1467,#1465,#132,.T.);
#1873=EDGE_CURVE('',#1464,#1466,#133,.T.);
#1874=EDGE_CURVE('',#1468,#1469,#900,.T.);
#1875=EDGE_CURVE('',#1469,#1467,#134,.T.);
#1876=EDGE_CURVE('',#1466,#1468,#135,.T.);
#1877=EDGE_CURVE('',#1470,#1471,#901,.T.);
#1878=EDGE_CURVE('',#1471,#1469,#136,.T.);
#1879=EDGE_CURVE('',#1468,#1470,#137,.T.);
#1880=EDGE_CURVE('',#1472,#1473,#902,.T.);
#1881=EDGE_CURVE('',#1473,#1471,#138,.T.);
#1882=EDGE_CURVE('',#1470,#1472,#139,.T.);
#1883=EDGE_CURVE('',#1474,#1475,#903,.T.);
#1884=EDGE_CURVE('',#1475,#1473,#140,.T.);
#1885=EDGE_CURVE('',#1472,#1474,#141,.T.);
#1886=EDGE_CURVE('',#1476,#1477,#904,.T.);
#1887=EDGE_CURVE('',#1476,#1478,#142,.T.);
#1888=EDGE_CURVE('',#1479,#1478,#1324,.T.);
#1889=EDGE_CURVE('',#1479,#1477,#143,.T.);
#1890=EDGE_CURVE('',#1480,#1481,#905,.T.);
#1891=EDGE_CURVE('',#1481,#1482,#144,.T.);
#1892=EDGE_CURVE('',#1483,#1482,#1325,.T.);
#1893=EDGE_CURVE('',#1480,#1483,#145,.T.);
#1894=EDGE_CURVE('',#1484,#1485,#906,.T.);
#1895=EDGE_CURVE('',#1485,#1481,#146,.T.);
#1896=EDGE_CURVE('',#1484,#1480,#147,.T.);
#1897=EDGE_CURVE('',#1486,#1487,#907,.T.);
#1898=EDGE_CURVE('',#1487,#1485,#148,.T.);
#1899=EDGE_CURVE('',#1486,#1484,#149,.T.);
#1900=EDGE_CURVE('',#1488,#1489,#908,.T.);
#1901=EDGE_CURVE('',#1489,#1487,#150,.T.);
#1902=EDGE_CURVE('',#1488,#1486,#151,.T.);
#1903=EDGE_CURVE('',#1490,#1491,#909,.T.);
#1904=EDGE_CURVE('',#1491,#1489,#152,.T.);
#1905=EDGE_CURVE('',#1490,#1488,#153,.T.);
#1906=EDGE_CURVE('',#1492,#1493,#910,.T.);
#1907=EDGE_CURVE('',#1493,#1491,#154,.T.);
#1908=EDGE_CURVE('',#1492,#1490,#155,.T.);
#1909=EDGE_CURVE('',#1494,#1495,#911,.T.);
#1910=EDGE_CURVE('',#1495,#1493,#156,.T.);
#1911=EDGE_CURVE('',#1494,#1492,#157,.T.);
#1912=EDGE_CURVE('',#1496,#1497,#912,.T.);
#1913=EDGE_CURVE('',#1497,#1495,#158,.T.);
#1914=EDGE_CURVE('',#1496,#1494,#159,.T.);
#1915=EDGE_CURVE('',#1498,#1499,#913,.T.);
#1916=EDGE_CURVE('',#1499,#1497,#160,.T.);
#1917=EDGE_CURVE('',#1498,#1496,#161,.T.);
#1918=EDGE_CURVE('',#1500,#1501,#914,.T.);
#1919=EDGE_CURVE('',#1501,#1499,#162,.T.);
#1920=EDGE_CURVE('',#1500,#1498,#163,.T.);
#1921=EDGE_CURVE('',#1502,#1503,#915,.T.);
#1922=EDGE_CURVE('',#1503,#1501,#164,.T.);
#1923=EDGE_CURVE('',#1502,#1500,#165,.T.);
#1924=EDGE_CURVE('',#1504,#1505,#916,.T.);
#1925=EDGE_CURVE('',#1505,#1503,#166,.T.);
#1926=EDGE_CURVE('',#1504,#1502,#167,.T.);
#1927=EDGE_CURVE('',#1506,#1507,#917,.T.);
#1928=EDGE_CURVE('',#1507,#1505,#168,.T.);
#1929=EDGE_CURVE('',#1506,#1504,#169,.T.);
#1930=EDGE_CURVE('',#1508,#1509,#918,.T.);
#1931=EDGE_CURVE('',#1510,#1508,#170,.T.);
#1932=EDGE_CURVE('',#1511,#1510,#1326,.T.);
#1933=EDGE_CURVE('',#1511,#1509,#171,.T.);
#1934=EDGE_CURVE('',#1512,#1512,#1327,.T.);
#1935=EDGE_CURVE('',#1512,#1513,#919,.T.);
#1936=EDGE_CURVE('',#1513,#1513,#1328,.T.);
#1937=EDGE_CURVE('',#1514,#1514,#1329,.T.);
#1938=EDGE_CURVE('',#1514,#1515,#920,.T.);
#1939=EDGE_CURVE('',#1515,#1515,#1330,.T.);
#1940=EDGE_CURVE('',#1450,#1483,#172,.T.);
#1941=EDGE_CURVE('',#1482,#1451,#173,.T.);
#1942=EDGE_CURVE('',#1509,#1507,#174,.T.);
#1943=EDGE_CURVE('',#1508,#1506,#175,.T.);
#1944=EDGE_CURVE('',#1478,#1511,#176,.T.);
#1945=EDGE_CURVE('',#1474,#1476,#177,.T.);
#1946=EDGE_CURVE('',#1477,#1475,#178,.T.);
#1947=EDGE_CURVE('',#1510,#1479,#179,.T.);
#1948=EDGE_CURVE('',#1386,#1419,#180,.T.);
#1949=EDGE_CURVE('',#1418,#1387,#181,.T.);
#1950=EDGE_CURVE('',#1445,#1443,#182,.T.);
#1951=EDGE_CURVE('',#1444,#1442,#183,.T.);
#1952=EDGE_CURVE('',#1414,#1447,#184,.T.);
#1953=EDGE_CURVE('',#1410,#1412,#185,.T.);
#1954=EDGE_CURVE('',#1413,#1411,#186,.T.);
#1955=EDGE_CURVE('',#1446,#1415,#187,.T.);
#1956=EDGE_CURVE('',#1516,#1517,#921,.T.);
#1957=EDGE_CURVE('',#1517,#1518,#922,.T.);
#1958=EDGE_CURVE('',#1519,#1518,#923,.T.);
#1959=EDGE_CURVE('',#1516,#1519,#924,.T.);
#1960=EDGE_CURVE('',#1520,#1516,#1331,.T.);
#1961=EDGE_CURVE('',#1521,#1519,#1332,.T.);
#1962=EDGE_CURVE('',#1520,#1521,#925,.T.);
#1963=EDGE_CURVE('',#1522,#1520,#926,.T.);
#1964=EDGE_CURVE('',#1523,#1521,#927,.T.);
#1965=EDGE_CURVE('',#1522,#1523,#928,.T.);
#1966=EDGE_CURVE('',#1524,#1522,#1333,.T.);
#1967=EDGE_CURVE('',#1525,#1523,#1334,.T.);
#1968=EDGE_CURVE('',#1524,#1525,#929,.T.);
#1969=EDGE_CURVE('',#1526,#1524,#930,.T.);
#1970=EDGE_CURVE('',#1527,#1525,#931,.T.);
#1971=EDGE_CURVE('',#1526,#1527,#932,.T.);
#1972=EDGE_CURVE('',#1528,#1526,#1335,.T.);
#1973=EDGE_CURVE('',#1529,#1527,#1336,.T.);
#1974=EDGE_CURVE('',#1528,#1529,#933,.T.);
#1975=EDGE_CURVE('',#1530,#1528,#934,.T.);
#1976=EDGE_CURVE('',#1531,#1529,#935,.T.);
#1977=EDGE_CURVE('',#1530,#1531,#936,.T.);
#1978=EDGE_CURVE('',#1517,#1530,#1337,.T.);
#1979=EDGE_CURVE('',#1518,#1531,#1338,.T.);
#1980=EDGE_CURVE('',#1532,#1533,#1339,.T.);
#1981=EDGE_CURVE('',#1532,#1534,#937,.T.);
#1982=EDGE_CURVE('',#1535,#1534,#1340,.T.);
#1983=EDGE_CURVE('',#1533,#1535,#938,.T.);
#1984=EDGE_CURVE('',#1536,#1533,#939,.T.);
#1985=EDGE_CURVE('',#1537,#1535,#940,.T.);
#1986=EDGE_CURVE('',#1536,#1537,#941,.T.);
#1987=EDGE_CURVE('',#1536,#1538,#1341,.T.);
#1988=EDGE_CURVE('',#1539,#1537,#1342,.T.);
#1989=EDGE_CURVE('',#1538,#1539,#942,.T.);
#1990=EDGE_CURVE('',#1540,#1538,#943,.T.);
#1991=EDGE_CURVE('',#1541,#1539,#944,.T.);
#1992=EDGE_CURVE('',#1540,#1541,#945,.T.);
#1993=EDGE_CURVE('',#1542,#1540,#946,.T.);
#1994=EDGE_CURVE('',#1543,#1541,#947,.T.);
#1995=EDGE_CURVE('',#1542,#1543,#948,.T.);
#1996=EDGE_CURVE('',#1544,#1542,#949,.T.);
#1997=EDGE_CURVE('',#1545,#1543,#950,.T.);
#1998=EDGE_CURVE('',#1544,#1545,#951,.T.);
#1999=EDGE_CURVE('',#1546,#1544,#952,.T.);
#2000=EDGE_CURVE('',#1547,#1545,#953,.T.);
#2001=EDGE_CURVE('',#1546,#1547,#954,.T.);
#2002=EDGE_CURVE('',#1548,#1546,#955,.T.);
#2003=EDGE_CURVE('',#1549,#1547,#956,.T.);
#2004=EDGE_CURVE('',#1548,#1549,#957,.T.);
#2005=EDGE_CURVE('',#1548,#1550,#1343,.T.);
#2006=EDGE_CURVE('',#1551,#1549,#1344,.T.);
#2007=EDGE_CURVE('',#1550,#1551,#958,.T.);
#2008=EDGE_CURVE('',#1552,#1550,#959,.T.);
#2009=EDGE_CURVE('',#1553,#1551,#960,.T.);
#2010=EDGE_CURVE('',#1552,#1553,#961,.T.);
#2011=EDGE_CURVE('',#1552,#1554,#1345,.T.);
#2012=EDGE_CURVE('',#1555,#1553,#1346,.T.);
#2013=EDGE_CURVE('',#1554,#1555,#962,.T.);
#2014=EDGE_CURVE('',#1556,#1554,#963,.T.);
#2015=EDGE_CURVE('',#1557,#1555,#964,.T.);
#2016=EDGE_CURVE('',#1556,#1557,#965,.T.);
#2017=EDGE_CURVE('',#1558,#1556,#966,.T.);
#2018=EDGE_CURVE('',#1559,#1557,#967,.T.);
#2019=EDGE_CURVE('',#1558,#1559,#968,.T.);
#2020=EDGE_CURVE('',#1560,#1558,#969,.T.);
#2021=EDGE_CURVE('',#1561,#1559,#970,.T.);
#2022=EDGE_CURVE('',#1560,#1561,#971,.T.);
#2023=EDGE_CURVE('',#1562,#1560,#972,.T.);
#2024=EDGE_CURVE('',#1563,#1561,#973,.T.);
#2025=EDGE_CURVE('',#1562,#1563,#974,.T.);
#2026=EDGE_CURVE('',#1532,#1562,#975,.T.);
#2027=EDGE_CURVE('',#1534,#1563,#976,.T.);
#2028=EDGE_CURVE('',#1564,#1565,#977,.T.);
#2029=EDGE_CURVE('',#1565,#1566,#978,.T.);
#2030=EDGE_CURVE('',#1567,#1566,#979,.T.);
#2031=EDGE_CURVE('',#1564,#1567,#980,.T.);
#2032=EDGE_CURVE('',#1568,#1564,#981,.T.);
#2033=EDGE_CURVE('',#1569,#1567,#982,.T.);
#2034=EDGE_CURVE('',#1568,#1569,#983,.T.);
#2035=EDGE_CURVE('',#1570,#1568,#984,.T.);
#2036=EDGE_CURVE('',#1571,#1569,#985,.T.);
#2037=EDGE_CURVE('',#1570,#1571,#986,.T.);
#2038=EDGE_CURVE('',#1565,#1570,#987,.T.);
#2039=EDGE_CURVE('',#1566,#1571,#988,.T.);
#2040=EDGE_CURVE('',#1572,#1572,#1347,.T.);
#2041=EDGE_CURVE('',#1572,#1573,#989,.T.);
#2042=EDGE_CURVE('',#1573,#1573,#1348,.T.);
#2043=EDGE_CURVE('',#1574,#1574,#1349,.T.);
#2044=EDGE_CURVE('',#1574,#1575,#990,.T.);
#2045=EDGE_CURVE('',#1575,#1575,#1350,.T.);
#2046=EDGE_CURVE('',#1576,#1577,#991,.T.);
#2047=EDGE_CURVE('',#1576,#1578,#188,.T.);
#2048=EDGE_CURVE('',#1578,#1579,#1351,.F.);
#2049=EDGE_CURVE('',#1579,#1577,#189,.T.);
#2050=EDGE_CURVE('',#1580,#1581,#992,.T.);
#2051=EDGE_CURVE('',#1580,#1576,#190,.T.);
#2052=EDGE_CURVE('',#1577,#1581,#191,.T.);
#2053=EDGE_CURVE('',#1582,#1583,#993,.T.);
#2054=EDGE_CURVE('',#1582,#1580,#192,.T.);
#2055=EDGE_CURVE('',#1581,#1583,#193,.T.);
#2056=EDGE_CURVE('',#1584,#1585,#994,.T.);
#2057=EDGE_CURVE('',#1584,#1582,#194,.T.);
#2058=EDGE_CURVE('',#1583,#1585,#195,.T.);
#2059=EDGE_CURVE('',#1586,#1587,#995,.T.);
#2060=EDGE_CURVE('',#1586,#1584,#196,.T.);
#2061=EDGE_CURVE('',#1585,#1587,#197,.T.);
#2062=EDGE_CURVE('',#1588,#1589,#996,.T.);
#2063=EDGE_CURVE('',#1588,#1586,#198,.T.);
#2064=EDGE_CURVE('',#1587,#1589,#199,.T.);
#2065=EDGE_CURVE('',#1590,#1591,#997,.T.);
#2066=EDGE_CURVE('',#1590,#1588,#200,.T.);
#2067=EDGE_CURVE('',#1589,#1591,#201,.T.);
#2068=EDGE_CURVE('',#1592,#1593,#998,.T.);
#2069=EDGE_CURVE('',#1592,#1590,#202,.T.);
#2070=EDGE_CURVE('',#1591,#1593,#203,.T.);
#2071=EDGE_CURVE('',#1594,#1595,#999,.T.);
#2072=EDGE_CURVE('',#1594,#1592,#204,.T.);
#2073=EDGE_CURVE('',#1593,#1595,#205,.T.);
#2074=EDGE_CURVE('',#1596,#1597,#1000,.T.);
#2075=EDGE_CURVE('',#1596,#1594,#206,.T.);
#2076=EDGE_CURVE('',#1595,#1597,#207,.T.);
#2077=EDGE_CURVE('',#1598,#1599,#1001,.T.);
#2078=EDGE_CURVE('',#1598,#1596,#208,.T.);
#2079=EDGE_CURVE('',#1597,#1599,#209,.T.);
#2080=EDGE_CURVE('',#1600,#1601,#1002,.T.);
#2081=EDGE_CURVE('',#1600,#1598,#210,.T.);
#2082=EDGE_CURVE('',#1599,#1601,#211,.T.);
#2083=EDGE_CURVE('',#1602,#1603,#1003,.T.);
#2084=EDGE_CURVE('',#1602,#1600,#212,.T.);
#2085=EDGE_CURVE('',#1601,#1603,#213,.T.);
#2086=EDGE_CURVE('',#1604,#1605,#1004,.T.);
#2087=EDGE_CURVE('',#1604,#1602,#214,.T.);
#2088=EDGE_CURVE('',#1603,#1605,#215,.T.);
#2089=EDGE_CURVE('',#1606,#1607,#1005,.T.);
#2090=EDGE_CURVE('',#1606,#1604,#216,.T.);
#2091=EDGE_CURVE('',#1605,#1607,#217,.T.);
#2092=EDGE_CURVE('',#1608,#1609,#1006,.T.);
#2093=EDGE_CURVE('',#1608,#1606,#218,.T.);
#2094=EDGE_CURVE('',#1607,#1609,#219,.T.);
#2095=EDGE_CURVE('',#1610,#1611,#1007,.T.);
#2096=EDGE_CURVE('',#1610,#1608,#220,.T.);
#2097=EDGE_CURVE('',#1609,#1611,#221,.T.);
#2098=EDGE_CURVE('',#1612,#1613,#1008,.T.);
#2099=EDGE_CURVE('',#1612,#1610,#222,.T.);
#2100=EDGE_CURVE('',#1611,#1613,#223,.T.);
#2101=EDGE_CURVE('',#1614,#1615,#1009,.T.);
#2102=EDGE_CURVE('',#1614,#1612,#224,.T.);
#2103=EDGE_CURVE('',#1613,#1615,#225,.T.);
#2104=EDGE_CURVE('',#1616,#1617,#1010,.T.);
#2105=EDGE_CURVE('',#1616,#1614,#226,.T.);
#2106=EDGE_CURVE('',#1615,#1617,#227,.T.);
#2107=EDGE_CURVE('',#1618,#1619,#1011,.T.);
#2108=EDGE_CURVE('',#1618,#1616,#228,.T.);
#2109=EDGE_CURVE('',#1617,#1619,#229,.T.);
#2110=EDGE_CURVE('',#1620,#1621,#1012,.T.);
#2111=EDGE_CURVE('',#1620,#1618,#230,.T.);
#2112=EDGE_CURVE('',#1619,#1621,#231,.T.);
#2113=EDGE_CURVE('',#1622,#1623,#1013,.T.);
#2114=EDGE_CURVE('',#1622,#1620,#232,.T.);
#2115=EDGE_CURVE('',#1621,#1623,#233,.T.);
#2116=EDGE_CURVE('',#1624,#1625,#1014,.T.);
#2117=EDGE_CURVE('',#1624,#1622,#234,.T.);
#2118=EDGE_CURVE('',#1623,#1625,#235,.T.);
#2119=EDGE_CURVE('',#1626,#1627,#1015,.T.);
#2120=EDGE_CURVE('',#1626,#1624,#236,.T.);
#2121=EDGE_CURVE('',#1625,#1627,#237,.T.);
#2122=EDGE_CURVE('',#1628,#1629,#1016,.T.);
#2123=EDGE_CURVE('',#1628,#1626,#238,.T.);
#2124=EDGE_CURVE('',#1627,#1629,#239,.T.);
#2125=EDGE_CURVE('',#1630,#1631,#1017,.T.);
#2126=EDGE_CURVE('',#1630,#1628,#240,.T.);
#2127=EDGE_CURVE('',#1629,#1631,#241,.T.);
#2128=EDGE_CURVE('',#1632,#1633,#1018,.T.);
#2129=EDGE_CURVE('',#1632,#1630,#242,.T.);
#2130=EDGE_CURVE('',#1631,#1633,#243,.T.);
#2131=EDGE_CURVE('',#1634,#1635,#1019,.T.);
#2132=EDGE_CURVE('',#1634,#1632,#244,.T.);
#2133=EDGE_CURVE('',#1633,#1635,#245,.T.);
#2134=EDGE_CURVE('',#1636,#1637,#1020,.T.);
#2135=EDGE_CURVE('',#1636,#1634,#246,.T.);
#2136=EDGE_CURVE('',#1635,#1637,#247,.T.);
#2137=EDGE_CURVE('',#1638,#1639,#1021,.T.);
#2138=EDGE_CURVE('',#1638,#1640,#248,.T.);
#2139=EDGE_CURVE('',#1640,#1641,#1352,.T.);
#2140=EDGE_CURVE('',#1639,#1641,#249,.T.);
#2141=EDGE_CURVE('',#1642,#1643,#1022,.T.);
#2142=EDGE_CURVE('',#1642,#1638,#250,.T.);
#2143=EDGE_CURVE('',#1643,#1639,#251,.T.);
#2144=EDGE_CURVE('',#1644,#1645,#1023,.T.);
#2145=EDGE_CURVE('',#1644,#1642,#252,.T.);
#2146=EDGE_CURVE('',#1645,#1643,#253,.T.);
#2147=EDGE_CURVE('',#1646,#1647,#1024,.T.);
#2148=EDGE_CURVE('',#1646,#1644,#254,.T.);
#2149=EDGE_CURVE('',#1647,#1645,#255,.T.);
#2150=EDGE_CURVE('',#1648,#1649,#1025,.T.);
#2151=EDGE_CURVE('',#1648,#1646,#256,.T.);
#2152=EDGE_CURVE('',#1649,#1647,#257,.T.);
#2153=EDGE_CURVE('',#1650,#1651,#1026,.T.);
#2154=EDGE_CURVE('',#1650,#1648,#258,.T.);
#2155=EDGE_CURVE('',#1651,#1649,#259,.T.);
#2156=EDGE_CURVE('',#1652,#1653,#1027,.T.);
#2157=EDGE_CURVE('',#1652,#1650,#260,.T.);
#2158=EDGE_CURVE('',#1653,#1651,#261,.T.);
#2159=EDGE_CURVE('',#1654,#1655,#1028,.T.);
#2160=EDGE_CURVE('',#1654,#1652,#262,.T.);
#2161=EDGE_CURVE('',#1655,#1653,#263,.T.);
#2162=EDGE_CURVE('',#1656,#1657,#1029,.T.);
#2163=EDGE_CURVE('',#1656,#1654,#264,.T.);
#2164=EDGE_CURVE('',#1657,#1655,#265,.T.);
#2165=EDGE_CURVE('',#1658,#1659,#1030,.T.);
#2166=EDGE_CURVE('',#1658,#1656,#266,.T.);
#2167=EDGE_CURVE('',#1659,#1657,#267,.T.);
#2168=EDGE_CURVE('',#1660,#1661,#1031,.T.);
#2169=EDGE_CURVE('',#1660,#1658,#268,.T.);
#2170=EDGE_CURVE('',#1661,#1659,#269,.T.);
#2171=EDGE_CURVE('',#1662,#1663,#1032,.T.);
#2172=EDGE_CURVE('',#1662,#1660,#270,.T.);
#2173=EDGE_CURVE('',#1663,#1661,#271,.T.);
#2174=EDGE_CURVE('',#1664,#1665,#1033,.T.);
#2175=EDGE_CURVE('',#1664,#1662,#272,.T.);
#2176=EDGE_CURVE('',#1665,#1663,#273,.T.);
#2177=EDGE_CURVE('',#1666,#1667,#1034,.T.);
#2178=EDGE_CURVE('',#1666,#1664,#274,.T.);
#2179=EDGE_CURVE('',#1667,#1665,#275,.T.);
#2180=EDGE_CURVE('',#1668,#1669,#1035,.T.);
#2181=EDGE_CURVE('',#1668,#1666,#276,.T.);
#2182=EDGE_CURVE('',#1669,#1667,#277,.T.);
#2183=EDGE_CURVE('',#1670,#1671,#1036,.T.);
#2184=EDGE_CURVE('',#1670,#1668,#278,.T.);
#2185=EDGE_CURVE('',#1671,#1669,#279,.T.);
#2186=EDGE_CURVE('',#1672,#1673,#1037,.T.);
#2187=EDGE_CURVE('',#1672,#1670,#280,.T.);
#2188=EDGE_CURVE('',#1673,#1671,#281,.T.);
#2189=EDGE_CURVE('',#1674,#1675,#1038,.T.);
#2190=EDGE_CURVE('',#1674,#1672,#282,.T.);
#2191=EDGE_CURVE('',#1675,#1673,#283,.T.);
#2192=EDGE_CURVE('',#1676,#1677,#1039,.T.);
#2193=EDGE_CURVE('',#1676,#1674,#284,.T.);
#2194=EDGE_CURVE('',#1677,#1675,#285,.T.);
#2195=EDGE_CURVE('',#1678,#1679,#1040,.T.);
#2196=EDGE_CURVE('',#1678,#1676,#286,.T.);
#2197=EDGE_CURVE('',#1679,#1677,#287,.T.);
#2198=EDGE_CURVE('',#1680,#1681,#1041,.T.);
#2199=EDGE_CURVE('',#1680,#1678,#288,.T.);
#2200=EDGE_CURVE('',#1681,#1679,#289,.T.);
#2201=EDGE_CURVE('',#1682,#1683,#1042,.T.);
#2202=EDGE_CURVE('',#1682,#1680,#290,.T.);
#2203=EDGE_CURVE('',#1683,#1681,#291,.T.);
#2204=EDGE_CURVE('',#1684,#1685,#1043,.T.);
#2205=EDGE_CURVE('',#1684,#1682,#292,.T.);
#2206=EDGE_CURVE('',#1685,#1683,#293,.T.);
#2207=EDGE_CURVE('',#1686,#1687,#1044,.T.);
#2208=EDGE_CURVE('',#1686,#1684,#294,.T.);
#2209=EDGE_CURVE('',#1687,#1685,#295,.T.);
#2210=EDGE_CURVE('',#1688,#1689,#1045,.T.);
#2211=EDGE_CURVE('',#1688,#1686,#296,.T.);
#2212=EDGE_CURVE('',#1689,#1687,#297,.T.);
#2213=EDGE_CURVE('',#1690,#1691,#1046,.T.);
#2214=EDGE_CURVE('',#1690,#1688,#298,.T.);
#2215=EDGE_CURVE('',#1691,#1689,#299,.T.);
#2216=EDGE_CURVE('',#1692,#1693,#1047,.T.);
#2217=EDGE_CURVE('',#1692,#1690,#300,.T.);
#2218=EDGE_CURVE('',#1693,#1691,#301,.T.);
#2219=EDGE_CURVE('',#1694,#1695,#1048,.T.);
#2220=EDGE_CURVE('',#1694,#1692,#302,.T.);
#2221=EDGE_CURVE('',#1695,#1693,#303,.T.);
#2222=EDGE_CURVE('',#1696,#1697,#1049,.T.);
#2223=EDGE_CURVE('',#1696,#1694,#304,.T.);
#2224=EDGE_CURVE('',#1697,#1695,#305,.T.);
#2225=EDGE_CURVE('',#1698,#1699,#1050,.T.);
#2226=EDGE_CURVE('',#1698,#1696,#306,.T.);
#2227=EDGE_CURVE('',#1699,#1697,#307,.T.);
#2228=EDGE_CURVE('',#1641,#1700,#308,.T.);
#2229=EDGE_CURVE('',#1701,#1640,#309,.T.);
#2230=EDGE_CURVE('',#1702,#1701,#1353,.T.);
#2231=EDGE_CURVE('',#1700,#1702,#310,.T.);
#2232=EDGE_CURVE('',#1700,#1703,#1051,.T.);
#2233=EDGE_CURVE('',#1703,#1703,#1354,.T.);
#2234=EDGE_CURVE('',#1704,#1698,#311,.T.);
#2235=EDGE_CURVE('',#1578,#1704,#312,.T.);
#2236=EDGE_CURVE('',#1701,#1636,#313,.T.);
#2237=EDGE_CURVE('',#1705,#1699,#314,.T.);
#2238=EDGE_CURVE('',#1704,#1705,#1355,.T.);
#2239=EDGE_CURVE('',#1637,#1702,#315,.T.);
#2240=EDGE_CURVE('',#1705,#1579,#316,.T.);
#2241=EDGE_CURVE('',#1706,#1707,#1052,.T.);
#2242=EDGE_CURVE('',#1706,#1708,#1053,.T.);
#2243=EDGE_CURVE('',#1708,#1709,#1054,.T.);
#2244=EDGE_CURVE('',#1707,#1709,#1055,.T.);
#2245=EDGE_CURVE('',#1710,#1706,#1056,.T.);
#2246=EDGE_CURVE('',#1710,#1711,#1057,.T.);
#2247=EDGE_CURVE('',#1711,#1708,#1058,.T.);
#2248=EDGE_CURVE('',#1712,#1710,#1059,.T.);
#2249=EDGE_CURVE('',#1712,#1713,#1060,.T.);
#2250=EDGE_CURVE('',#1713,#1711,#1061,.T.);
#2251=EDGE_CURVE('',#1714,#1712,#1062,.T.);
#2252=EDGE_CURVE('',#1714,#1715,#1063,.T.);
#2253=EDGE_CURVE('',#1715,#1713,#1064,.T.);
#2254=EDGE_CURVE('',#1716,#1714,#1065,.T.);
#2255=EDGE_CURVE('',#1716,#1717,#1066,.T.);
#2256=EDGE_CURVE('',#1717,#1715,#1067,.T.);
#2257=EDGE_CURVE('',#1707,#1716,#1068,.T.);
#2258=EDGE_CURVE('',#1709,#1717,#1069,.T.);
#2259=EDGE_CURVE('',#1718,#1718,#1356,.T.);
#2260=EDGE_CURVE('',#1718,#1719,#1070,.T.);
#2261=EDGE_CURVE('',#1719,#1719,#1357,.T.);
#2262=EDGE_CURVE('',#1720,#1720,#1358,.T.);
#2263=EDGE_CURVE('',#1720,#1721,#1071,.T.);
#2264=EDGE_CURVE('',#1721,#1721,#1359,.T.);
#2265=ORIENTED_EDGE('',*,*,#1722,.F.);
#2266=ORIENTED_EDGE('',*,*,#1723,.T.);
#2267=ORIENTED_EDGE('',*,*,#1724,.T.);
#2268=ORIENTED_EDGE('',*,*,#1723,.F.);
#2269=ORIENTED_EDGE('',*,*,#1724,.F.);
#2270=ORIENTED_EDGE('',*,*,#1725,.F.);
#2271=ORIENTED_EDGE('',*,*,#1726,.T.);
#2272=ORIENTED_EDGE('',*,*,#1727,.T.);
#2273=ORIENTED_EDGE('',*,*,#1726,.F.);
#2274=ORIENTED_EDGE('',*,*,#1727,.F.);
#2275=ORIENTED_EDGE('',*,*,#1728,.F.);
#2276=ORIENTED_EDGE('',*,*,#1729,.T.);
#2277=ORIENTED_EDGE('',*,*,#1730,.F.);
#2278=ORIENTED_EDGE('',*,*,#1729,.F.);
#2279=ORIENTED_EDGE('',*,*,#1731,.F.);
#2280=ORIENTED_EDGE('',*,*,#1732,.T.);
#2281=ORIENTED_EDGE('',*,*,#1733,.F.);
#2282=ORIENTED_EDGE('',*,*,#1732,.F.);
#2283=ORIENTED_EDGE('',*,*,#1734,.F.);
#2284=ORIENTED_EDGE('',*,*,#1735,.T.);
#2285=ORIENTED_EDGE('',*,*,#1736,.F.);
#2286=ORIENTED_EDGE('',*,*,#1735,.F.);
#2287=ORIENTED_EDGE('',*,*,#1737,.F.);
#2288=ORIENTED_EDGE('',*,*,#1738,.T.);
#2289=ORIENTED_EDGE('',*,*,#1739,.F.);
#2290=ORIENTED_EDGE('',*,*,#1738,.F.);
#2291=ORIENTED_EDGE('',*,*,#1740,.F.);
#2292=ORIENTED_EDGE('',*,*,#1741,.T.);
#2293=ORIENTED_EDGE('',*,*,#1742,.F.);
#2294=ORIENTED_EDGE('',*,*,#1741,.F.);
#2295=ORIENTED_EDGE('',*,*,#1743,.F.);
#2296=ORIENTED_EDGE('',*,*,#1744,.T.);
#2297=ORIENTED_EDGE('',*,*,#1745,.F.);
#2298=ORIENTED_EDGE('',*,*,#1744,.F.);
#2299=ORIENTED_EDGE('',*,*,#1746,.T.);
#2300=ORIENTED_EDGE('',*,*,#1747,.T.);
#2301=ORIENTED_EDGE('',*,*,#1748,.F.);
#2302=ORIENTED_EDGE('',*,*,#1749,.F.);
#2303=ORIENTED_EDGE('',*,*,#1750,.T.);
#2304=ORIENTED_EDGE('',*,*,#1749,.T.);
#2305=ORIENTED_EDGE('',*,*,#1751,.F.);
#2306=ORIENTED_EDGE('',*,*,#1752,.F.);
#2307=ORIENTED_EDGE('',*,*,#1730,.T.);
#2308=ORIENTED_EDGE('',*,*,#1733,.T.);
#2309=ORIENTED_EDGE('',*,*,#1736,.T.);
#2310=ORIENTED_EDGE('',*,*,#1739,.T.);
#2311=ORIENTED_EDGE('',*,*,#1742,.T.);
#2312=ORIENTED_EDGE('',*,*,#1745,.T.);
#2313=ORIENTED_EDGE('',*,*,#1725,.T.);
#2314=ORIENTED_EDGE('',*,*,#1722,.T.);
#2315=ORIENTED_EDGE('',*,*,#1753,.T.);
#2316=ORIENTED_EDGE('',*,*,#1752,.T.);
#2317=ORIENTED_EDGE('',*,*,#1754,.F.);
#2318=ORIENTED_EDGE('',*,*,#1755,.F.);
#2319=ORIENTED_EDGE('',*,*,#1756,.T.);
#2320=ORIENTED_EDGE('',*,*,#1755,.T.);
#2321=ORIENTED_EDGE('',*,*,#1757,.F.);
#2322=ORIENTED_EDGE('',*,*,#1747,.F.);
#2323=ORIENTED_EDGE('',*,*,#1743,.T.);
#2324=ORIENTED_EDGE('',*,*,#1740,.T.);
#2325=ORIENTED_EDGE('',*,*,#1737,.T.);
#2326=ORIENTED_EDGE('',*,*,#1734,.T.);
#2327=ORIENTED_EDGE('',*,*,#1731,.T.);
#2328=ORIENTED_EDGE('',*,*,#1728,.T.);
#2329=ORIENTED_EDGE('',*,*,#1757,.T.);
#2330=ORIENTED_EDGE('',*,*,#1754,.T.);
#2331=ORIENTED_EDGE('',*,*,#1751,.T.);
#2332=ORIENTED_EDGE('',*,*,#1748,.T.);
#2333=ORIENTED_EDGE('',*,*,#1756,.F.);
#2334=ORIENTED_EDGE('',*,*,#1746,.F.);
#2335=ORIENTED_EDGE('',*,*,#1750,.F.);
#2336=ORIENTED_EDGE('',*,*,#1753,.F.);
#2337=ORIENTED_EDGE('',*,*,#1758,.T.);
#2338=ORIENTED_EDGE('',*,*,#1759,.T.);
#2339=ORIENTED_EDGE('',*,*,#1760,.T.);
#2340=ORIENTED_EDGE('',*,*,#1761,.T.);
#2341=ORIENTED_EDGE('',*,*,#1762,.T.);
#2342=ORIENTED_EDGE('',*,*,#1763,.T.);
#2343=ORIENTED_EDGE('',*,*,#1762,.F.);
#2344=ORIENTED_EDGE('',*,*,#1764,.T.);
#2345=ORIENTED_EDGE('',*,*,#1765,.T.);
#2346=ORIENTED_EDGE('',*,*,#1766,.T.);
#2347=ORIENTED_EDGE('',*,*,#1758,.F.);
#2348=ORIENTED_EDGE('',*,*,#1767,.T.);
#2349=ORIENTED_EDGE('',*,*,#1768,.T.);
#2350=ORIENTED_EDGE('',*,*,#1769,.T.);
#2351=ORIENTED_EDGE('',*,*,#1765,.F.);
#2352=ORIENTED_EDGE('',*,*,#1770,.T.);
#2353=ORIENTED_EDGE('',*,*,#1771,.T.);
#2354=ORIENTED_EDGE('',*,*,#1772,.T.);
#2355=ORIENTED_EDGE('',*,*,#1768,.F.);
#2356=ORIENTED_EDGE('',*,*,#1773,.T.);
#2357=ORIENTED_EDGE('',*,*,#1774,.T.);
#2358=ORIENTED_EDGE('',*,*,#1775,.T.);
#2359=ORIENTED_EDGE('',*,*,#1771,.F.);
#2360=ORIENTED_EDGE('',*,*,#1776,.T.);
#2361=ORIENTED_EDGE('',*,*,#1777,.T.);
#2362=ORIENTED_EDGE('',*,*,#1778,.T.);
#2363=ORIENTED_EDGE('',*,*,#1774,.F.);
#2364=ORIENTED_EDGE('',*,*,#1779,.T.);
#2365=ORIENTED_EDGE('',*,*,#1780,.T.);
#2366=ORIENTED_EDGE('',*,*,#1781,.T.);
#2367=ORIENTED_EDGE('',*,*,#1777,.F.);
#2368=ORIENTED_EDGE('',*,*,#1782,.T.);
#2369=ORIENTED_EDGE('',*,*,#1783,.T.);
#2370=ORIENTED_EDGE('',*,*,#1784,.T.);
#2371=ORIENTED_EDGE('',*,*,#1780,.F.);
#2372=ORIENTED_EDGE('',*,*,#1785,.T.);
#2373=ORIENTED_EDGE('',*,*,#1786,.T.);
#2374=ORIENTED_EDGE('',*,*,#1787,.T.);
#2375=ORIENTED_EDGE('',*,*,#1783,.F.);
#2376=ORIENTED_EDGE('',*,*,#1788,.T.);
#2377=ORIENTED_EDGE('',*,*,#1789,.T.);
#2378=ORIENTED_EDGE('',*,*,#1790,.T.);
#2379=ORIENTED_EDGE('',*,*,#1786,.F.);
#2380=ORIENTED_EDGE('',*,*,#1791,.T.);
#2381=ORIENTED_EDGE('',*,*,#1792,.T.);
#2382=ORIENTED_EDGE('',*,*,#1793,.T.);
#2383=ORIENTED_EDGE('',*,*,#1789,.F.);
#2384=ORIENTED_EDGE('',*,*,#1794,.T.);
#2385=ORIENTED_EDGE('',*,*,#1795,.T.);
#2386=ORIENTED_EDGE('',*,*,#1796,.T.);
#2387=ORIENTED_EDGE('',*,*,#1792,.F.);
#2388=ORIENTED_EDGE('',*,*,#1797,.T.);
#2389=ORIENTED_EDGE('',*,*,#1798,.F.);
#2390=ORIENTED_EDGE('',*,*,#1799,.T.);
#2391=ORIENTED_EDGE('',*,*,#1800,.F.);
#2392=ORIENTED_EDGE('',*,*,#1801,.T.);
#2393=ORIENTED_EDGE('',*,*,#1802,.T.);
#2394=ORIENTED_EDGE('',*,*,#1803,.T.);
#2395=ORIENTED_EDGE('',*,*,#1804,.F.);
#2396=ORIENTED_EDGE('',*,*,#1805,.F.);
#2397=ORIENTED_EDGE('',*,*,#1806,.T.);
#2398=ORIENTED_EDGE('',*,*,#1807,.T.);
#2399=ORIENTED_EDGE('',*,*,#1802,.F.);
#2400=ORIENTED_EDGE('',*,*,#1808,.F.);
#2401=ORIENTED_EDGE('',*,*,#1809,.T.);
#2402=ORIENTED_EDGE('',*,*,#1810,.T.);
#2403=ORIENTED_EDGE('',*,*,#1806,.F.);
#2404=ORIENTED_EDGE('',*,*,#1811,.F.);
#2405=ORIENTED_EDGE('',*,*,#1812,.T.);
#2406=ORIENTED_EDGE('',*,*,#1813,.T.);
#2407=ORIENTED_EDGE('',*,*,#1809,.F.);
#2408=ORIENTED_EDGE('',*,*,#1814,.F.);
#2409=ORIENTED_EDGE('',*,*,#1815,.T.);
#2410=ORIENTED_EDGE('',*,*,#1816,.T.);
#2411=ORIENTED_EDGE('',*,*,#1812,.F.);
#2412=ORIENTED_EDGE('',*,*,#1817,.F.);
#2413=ORIENTED_EDGE('',*,*,#1818,.T.);
#2414=ORIENTED_EDGE('',*,*,#1819,.T.);
#2415=ORIENTED_EDGE('',*,*,#1815,.F.);
#2416=ORIENTED_EDGE('',*,*,#1820,.F.);
#2417=ORIENTED_EDGE('',*,*,#1821,.T.);
#2418=ORIENTED_EDGE('',*,*,#1822,.T.);
#2419=ORIENTED_EDGE('',*,*,#1818,.F.);
#2420=ORIENTED_EDGE('',*,*,#1823,.F.);
#2421=ORIENTED_EDGE('',*,*,#1824,.T.);
#2422=ORIENTED_EDGE('',*,*,#1825,.T.);
#2423=ORIENTED_EDGE('',*,*,#1821,.F.);
#2424=ORIENTED_EDGE('',*,*,#1826,.F.);
#2425=ORIENTED_EDGE('',*,*,#1827,.T.);
#2426=ORIENTED_EDGE('',*,*,#1828,.T.);
#2427=ORIENTED_EDGE('',*,*,#1824,.F.);
#2428=ORIENTED_EDGE('',*,*,#1829,.F.);
#2429=ORIENTED_EDGE('',*,*,#1830,.T.);
#2430=ORIENTED_EDGE('',*,*,#1831,.T.);
#2431=ORIENTED_EDGE('',*,*,#1827,.F.);
#2432=ORIENTED_EDGE('',*,*,#1832,.F.);
#2433=ORIENTED_EDGE('',*,*,#1833,.T.);
#2434=ORIENTED_EDGE('',*,*,#1834,.T.);
#2435=ORIENTED_EDGE('',*,*,#1830,.F.);
#2436=ORIENTED_EDGE('',*,*,#1835,.F.);
#2437=ORIENTED_EDGE('',*,*,#1836,.T.);
#2438=ORIENTED_EDGE('',*,*,#1837,.T.);
#2439=ORIENTED_EDGE('',*,*,#1833,.F.);
#2440=ORIENTED_EDGE('',*,*,#1838,.F.);
#2441=ORIENTED_EDGE('',*,*,#1839,.T.);
#2442=ORIENTED_EDGE('',*,*,#1840,.T.);
#2443=ORIENTED_EDGE('',*,*,#1836,.F.);
#2444=ORIENTED_EDGE('',*,*,#1841,.F.);
#2445=ORIENTED_EDGE('',*,*,#1842,.F.);
#2446=ORIENTED_EDGE('',*,*,#1843,.F.);
#2447=ORIENTED_EDGE('',*,*,#1844,.F.);
#2448=ORIENTED_EDGE('',*,*,#1845,.T.);
#2449=ORIENTED_EDGE('',*,*,#1846,.T.);
#2450=ORIENTED_EDGE('',*,*,#1847,.T.);
#2451=ORIENTED_EDGE('',*,*,#1848,.T.);
#2452=ORIENTED_EDGE('',*,*,#1849,.T.);
#2453=ORIENTED_EDGE('',*,*,#1850,.T.);
#2454=ORIENTED_EDGE('',*,*,#1851,.T.);
#2455=ORIENTED_EDGE('',*,*,#1850,.F.);
#2456=ORIENTED_EDGE('',*,*,#1852,.T.);
#2457=ORIENTED_EDGE('',*,*,#1853,.T.);
#2458=ORIENTED_EDGE('',*,*,#1854,.T.);
#2459=ORIENTED_EDGE('',*,*,#1846,.F.);
#2460=ORIENTED_EDGE('',*,*,#1855,.T.);
#2461=ORIENTED_EDGE('',*,*,#1856,.T.);
#2462=ORIENTED_EDGE('',*,*,#1857,.T.);
#2463=ORIENTED_EDGE('',*,*,#1853,.F.);
#2464=ORIENTED_EDGE('',*,*,#1858,.T.);
#2465=ORIENTED_EDGE('',*,*,#1859,.T.);
#2466=ORIENTED_EDGE('',*,*,#1860,.T.);
#2467=ORIENTED_EDGE('',*,*,#1856,.F.);
#2468=ORIENTED_EDGE('',*,*,#1861,.T.);
#2469=ORIENTED_EDGE('',*,*,#1862,.T.);
#2470=ORIENTED_EDGE('',*,*,#1863,.T.);
#2471=ORIENTED_EDGE('',*,*,#1859,.F.);
#2472=ORIENTED_EDGE('',*,*,#1864,.T.);
#2473=ORIENTED_EDGE('',*,*,#1865,.T.);
#2474=ORIENTED_EDGE('',*,*,#1866,.T.);
#2475=ORIENTED_EDGE('',*,*,#1862,.F.);
#2476=ORIENTED_EDGE('',*,*,#1867,.T.);
#2477=ORIENTED_EDGE('',*,*,#1868,.T.);
#2478=ORIENTED_EDGE('',*,*,#1869,.T.);
#2479=ORIENTED_EDGE('',*,*,#1865,.F.);
#2480=ORIENTED_EDGE('',*,*,#1870,.T.);
#2481=ORIENTED_EDGE('',*,*,#1871,.T.);
#2482=ORIENTED_EDGE('',*,*,#1872,.T.);
#2483=ORIENTED_EDGE('',*,*,#1868,.F.);
#2484=ORIENTED_EDGE('',*,*,#1873,.T.);
#2485=ORIENTED_EDGE('',*,*,#1874,.T.);
#2486=ORIENTED_EDGE('',*,*,#1875,.T.);
#2487=ORIENTED_EDGE('',*,*,#1871,.F.);
#2488=ORIENTED_EDGE('',*,*,#1876,.T.);
#2489=ORIENTED_EDGE('',*,*,#1877,.T.);
#2490=ORIENTED_EDGE('',*,*,#1878,.T.);
#2491=ORIENTED_EDGE('',*,*,#1874,.F.);
#2492=ORIENTED_EDGE('',*,*,#1879,.T.);
#2493=ORIENTED_EDGE('',*,*,#1880,.T.);
#2494=ORIENTED_EDGE('',*,*,#1881,.T.);
#2495=ORIENTED_EDGE('',*,*,#1877,.F.);
#2496=ORIENTED_EDGE('',*,*,#1882,.T.);
#2497=ORIENTED_EDGE('',*,*,#1883,.T.);
#2498=ORIENTED_EDGE('',*,*,#1884,.T.);
#2499=ORIENTED_EDGE('',*,*,#1880,.F.);
#2500=ORIENTED_EDGE('',*,*,#1885,.T.);
#2501=ORIENTED_EDGE('',*,*,#1886,.F.);
#2502=ORIENTED_EDGE('',*,*,#1887,.T.);
#2503=ORIENTED_EDGE('',*,*,#1888,.F.);
#2504=ORIENTED_EDGE('',*,*,#1889,.T.);
#2505=ORIENTED_EDGE('',*,*,#1890,.T.);
#2506=ORIENTED_EDGE('',*,*,#1891,.T.);
#2507=ORIENTED_EDGE('',*,*,#1892,.F.);
#2508=ORIENTED_EDGE('',*,*,#1893,.F.);
#2509=ORIENTED_EDGE('',*,*,#1894,.T.);
#2510=ORIENTED_EDGE('',*,*,#1895,.T.);
#2511=ORIENTED_EDGE('',*,*,#1890,.F.);
#2512=ORIENTED_EDGE('',*,*,#1896,.F.);
#2513=ORIENTED_EDGE('',*,*,#1897,.T.);
#2514=ORIENTED_EDGE('',*,*,#1898,.T.);
#2515=ORIENTED_EDGE('',*,*,#1894,.F.);
#2516=ORIENTED_EDGE('',*,*,#1899,.F.);
#2517=ORIENTED_EDGE('',*,*,#1900,.T.);
#2518=ORIENTED_EDGE('',*,*,#1901,.T.);
#2519=ORIENTED_EDGE('',*,*,#1897,.F.);
#2520=ORIENTED_EDGE('',*,*,#1902,.F.);
#2521=ORIENTED_EDGE('',*,*,#1903,.T.);
#2522=ORIENTED_EDGE('',*,*,#1904,.T.);
#2523=ORIENTED_EDGE('',*,*,#1900,.F.);
#2524=ORIENTED_EDGE('',*,*,#1905,.F.);
#2525=ORIENTED_EDGE('',*,*,#1906,.T.);
#2526=ORIENTED_EDGE('',*,*,#1907,.T.);
#2527=ORIENTED_EDGE('',*,*,#1903,.F.);
#2528=ORIENTED_EDGE('',*,*,#1908,.F.);
#2529=ORIENTED_EDGE('',*,*,#1909,.T.);
#2530=ORIENTED_EDGE('',*,*,#1910,.T.);
#2531=ORIENTED_EDGE('',*,*,#1906,.F.);
#2532=ORIENTED_EDGE('',*,*,#1911,.F.);
#2533=ORIENTED_EDGE('',*,*,#1912,.T.);
#2534=ORIENTED_EDGE('',*,*,#1913,.T.);
#2535=ORIENTED_EDGE('',*,*,#1909,.F.);
#2536=ORIENTED_EDGE('',*,*,#1914,.F.);
#2537=ORIENTED_EDGE('',*,*,#1915,.T.);
#2538=ORIENTED_EDGE('',*,*,#1916,.T.);
#2539=ORIENTED_EDGE('',*,*,#1912,.F.);
#2540=ORIENTED_EDGE('',*,*,#1917,.F.);
#2541=ORIENTED_EDGE('',*,*,#1918,.T.);
#2542=ORIENTED_EDGE('',*,*,#1919,.T.);
#2543=ORIENTED_EDGE('',*,*,#1915,.F.);
#2544=ORIENTED_EDGE('',*,*,#1920,.F.);
#2545=ORIENTED_EDGE('',*,*,#1921,.T.);
#2546=ORIENTED_EDGE('',*,*,#1922,.T.);
#2547=ORIENTED_EDGE('',*,*,#1918,.F.);
#2548=ORIENTED_EDGE('',*,*,#1923,.F.);
#2549=ORIENTED_EDGE('',*,*,#1924,.T.);
#2550=ORIENTED_EDGE('',*,*,#1925,.T.);
#2551=ORIENTED_EDGE('',*,*,#1921,.F.);
#2552=ORIENTED_EDGE('',*,*,#1926,.F.);
#2553=ORIENTED_EDGE('',*,*,#1927,.T.);
#2554=ORIENTED_EDGE('',*,*,#1928,.T.);
#2555=ORIENTED_EDGE('',*,*,#1924,.F.);
#2556=ORIENTED_EDGE('',*,*,#1929,.F.);
#2557=ORIENTED_EDGE('',*,*,#1930,.F.);
#2558=ORIENTED_EDGE('',*,*,#1931,.F.);
#2559=ORIENTED_EDGE('',*,*,#1932,.F.);
#2560=ORIENTED_EDGE('',*,*,#1933,.T.);
#2561=ORIENTED_EDGE('',*,*,#1934,.F.);
#2562=ORIENTED_EDGE('',*,*,#1935,.T.);
#2563=ORIENTED_EDGE('',*,*,#1936,.T.);
#2564=ORIENTED_EDGE('',*,*,#1935,.F.);
#2565=ORIENTED_EDGE('',*,*,#1936,.F.);
#2566=ORIENTED_EDGE('',*,*,#1937,.F.);
#2567=ORIENTED_EDGE('',*,*,#1938,.T.);
#2568=ORIENTED_EDGE('',*,*,#1939,.T.);
#2569=ORIENTED_EDGE('',*,*,#1938,.F.);
#2570=ORIENTED_EDGE('',*,*,#1939,.F.);
#2571=ORIENTED_EDGE('',*,*,#1848,.F.);
#2572=ORIENTED_EDGE('',*,*,#1940,.T.);
#2573=ORIENTED_EDGE('',*,*,#1892,.T.);
#2574=ORIENTED_EDGE('',*,*,#1941,.T.);
#2575=ORIENTED_EDGE('',*,*,#1930,.T.);
#2576=ORIENTED_EDGE('',*,*,#1942,.T.);
#2577=ORIENTED_EDGE('',*,*,#1927,.F.);
#2578=ORIENTED_EDGE('',*,*,#1943,.F.);
#2579=ORIENTED_EDGE('',*,*,#1941,.F.);
#2580=ORIENTED_EDGE('',*,*,#1891,.F.);
#2581=ORIENTED_EDGE('',*,*,#1895,.F.);
#2582=ORIENTED_EDGE('',*,*,#1898,.F.);
#2583=ORIENTED_EDGE('',*,*,#1901,.F.);
#2584=ORIENTED_EDGE('',*,*,#1904,.F.);
#2585=ORIENTED_EDGE('',*,*,#1907,.F.);
#2586=ORIENTED_EDGE('',*,*,#1910,.F.);
#2587=ORIENTED_EDGE('',*,*,#1913,.F.);
#2588=ORIENTED_EDGE('',*,*,#1916,.F.);
#2589=ORIENTED_EDGE('',*,*,#1919,.F.);
#2590=ORIENTED_EDGE('',*,*,#1922,.F.);
#2591=ORIENTED_EDGE('',*,*,#1925,.F.);
#2592=ORIENTED_EDGE('',*,*,#1928,.F.);
#2593=ORIENTED_EDGE('',*,*,#1942,.F.);
#2594=ORIENTED_EDGE('',*,*,#1933,.F.);
#2595=ORIENTED_EDGE('',*,*,#1944,.F.);
#2596=ORIENTED_EDGE('',*,*,#1887,.F.);
#2597=ORIENTED_EDGE('',*,*,#1945,.F.);
#2598=ORIENTED_EDGE('',*,*,#1885,.F.);
#2599=ORIENTED_EDGE('',*,*,#1882,.F.);
#2600=ORIENTED_EDGE('',*,*,#1879,.F.);
#2601=ORIENTED_EDGE('',*,*,#1876,.F.);
#2602=ORIENTED_EDGE('',*,*,#1873,.F.);
#2603=ORIENTED_EDGE('',*,*,#1870,.F.);
#2604=ORIENTED_EDGE('',*,*,#1867,.F.);
#2605=ORIENTED_EDGE('',*,*,#1864,.F.);
#2606=ORIENTED_EDGE('',*,*,#1861,.F.);
#2607=ORIENTED_EDGE('',*,*,#1858,.F.);
#2608=ORIENTED_EDGE('',*,*,#1855,.F.);
#2609=ORIENTED_EDGE('',*,*,#1852,.F.);
#2610=ORIENTED_EDGE('',*,*,#1849,.F.);
#2611=ORIENTED_EDGE('',*,*,#1940,.F.);
#2612=ORIENTED_EDGE('',*,*,#1847,.F.);
#2613=ORIENTED_EDGE('',*,*,#1854,.F.);
#2614=ORIENTED_EDGE('',*,*,#1857,.F.);
#2615=ORIENTED_EDGE('',*,*,#1860,.F.);
#2616=ORIENTED_EDGE('',*,*,#1863,.F.);
#2617=ORIENTED_EDGE('',*,*,#1866,.F.);
#2618=ORIENTED_EDGE('',*,*,#1869,.F.);
#2619=ORIENTED_EDGE('',*,*,#1872,.F.);
#2620=ORIENTED_EDGE('',*,*,#1875,.F.);
#2621=ORIENTED_EDGE('',*,*,#1878,.F.);
#2622=ORIENTED_EDGE('',*,*,#1881,.F.);
#2623=ORIENTED_EDGE('',*,*,#1884,.F.);
#2624=ORIENTED_EDGE('',*,*,#1946,.F.);
#2625=ORIENTED_EDGE('',*,*,#1889,.F.);
#2626=ORIENTED_EDGE('',*,*,#1947,.F.);
#2627=ORIENTED_EDGE('',*,*,#1931,.T.);
#2628=ORIENTED_EDGE('',*,*,#1943,.T.);
#2629=ORIENTED_EDGE('',*,*,#1929,.T.);
#2630=ORIENTED_EDGE('',*,*,#1926,.T.);
#2631=ORIENTED_EDGE('',*,*,#1923,.T.);
#2632=ORIENTED_EDGE('',*,*,#1920,.T.);
#2633=ORIENTED_EDGE('',*,*,#1917,.T.);
#2634=ORIENTED_EDGE('',*,*,#1914,.T.);
#2635=ORIENTED_EDGE('',*,*,#1911,.T.);
#2636=ORIENTED_EDGE('',*,*,#1908,.T.);
#2637=ORIENTED_EDGE('',*,*,#1905,.T.);
#2638=ORIENTED_EDGE('',*,*,#1902,.T.);
#2639=ORIENTED_EDGE('',*,*,#1899,.T.);
#2640=ORIENTED_EDGE('',*,*,#1896,.T.);
#2641=ORIENTED_EDGE('',*,*,#1893,.T.);
#2642=ORIENTED_EDGE('',*,*,#1886,.T.);
#2643=ORIENTED_EDGE('',*,*,#1946,.T.);
#2644=ORIENTED_EDGE('',*,*,#1883,.F.);
#2645=ORIENTED_EDGE('',*,*,#1945,.T.);
#2646=ORIENTED_EDGE('',*,*,#1760,.F.);
#2647=ORIENTED_EDGE('',*,*,#1948,.T.);
#2648=ORIENTED_EDGE('',*,*,#1804,.T.);
#2649=ORIENTED_EDGE('',*,*,#1949,.T.);
#2650=ORIENTED_EDGE('',*,*,#1842,.T.);
#2651=ORIENTED_EDGE('',*,*,#1950,.T.);
#2652=ORIENTED_EDGE('',*,*,#1839,.F.);
#2653=ORIENTED_EDGE('',*,*,#1951,.F.);
#2654=ORIENTED_EDGE('',*,*,#1949,.F.);
#2655=ORIENTED_EDGE('',*,*,#1803,.F.);
#2656=ORIENTED_EDGE('',*,*,#1807,.F.);
#2657=ORIENTED_EDGE('',*,*,#1810,.F.);
#2658=ORIENTED_EDGE('',*,*,#1813,.F.);
#2659=ORIENTED_EDGE('',*,*,#1816,.F.);
#2660=ORIENTED_EDGE('',*,*,#1819,.F.);
#2661=ORIENTED_EDGE('',*,*,#1822,.F.);
#2662=ORIENTED_EDGE('',*,*,#1825,.F.);
#2663=ORIENTED_EDGE('',*,*,#1828,.F.);
#2664=ORIENTED_EDGE('',*,*,#1831,.F.);
#2665=ORIENTED_EDGE('',*,*,#1834,.F.);
#2666=ORIENTED_EDGE('',*,*,#1837,.F.);
#2667=ORIENTED_EDGE('',*,*,#1840,.F.);
#2668=ORIENTED_EDGE('',*,*,#1950,.F.);
#2669=ORIENTED_EDGE('',*,*,#1845,.F.);
#2670=ORIENTED_EDGE('',*,*,#1952,.F.);
#2671=ORIENTED_EDGE('',*,*,#1799,.F.);
#2672=ORIENTED_EDGE('',*,*,#1953,.F.);
#2673=ORIENTED_EDGE('',*,*,#1797,.F.);
#2674=ORIENTED_EDGE('',*,*,#1794,.F.);
#2675=ORIENTED_EDGE('',*,*,#1791,.F.);
#2676=ORIENTED_EDGE('',*,*,#1788,.F.);
#2677=ORIENTED_EDGE('',*,*,#1785,.F.);
#2678=ORIENTED_EDGE('',*,*,#1782,.F.);
#2679=ORIENTED_EDGE('',*,*,#1779,.F.);
#2680=ORIENTED_EDGE('',*,*,#1776,.F.);
#2681=ORIENTED_EDGE('',*,*,#1773,.F.);
#2682=ORIENTED_EDGE('',*,*,#1770,.F.);
#2683=ORIENTED_EDGE('',*,*,#1767,.F.);
#2684=ORIENTED_EDGE('',*,*,#1764,.F.);
#2685=ORIENTED_EDGE('',*,*,#1761,.F.);
#2686=ORIENTED_EDGE('',*,*,#1948,.F.);
#2687=ORIENTED_EDGE('',*,*,#1759,.F.);
#2688=ORIENTED_EDGE('',*,*,#1766,.F.);
#2689=ORIENTED_EDGE('',*,*,#1769,.F.);
#2690=ORIENTED_EDGE('',*,*,#1772,.F.);
#2691=ORIENTED_EDGE('',*,*,#1775,.F.);
#2692=ORIENTED_EDGE('',*,*,#1778,.F.);
#2693=ORIENTED_EDGE('',*,*,#1781,.F.);
#2694=ORIENTED_EDGE('',*,*,#1784,.F.);
#2695=ORIENTED_EDGE('',*,*,#1787,.F.);
#2696=ORIENTED_EDGE('',*,*,#1790,.F.);
#2697=ORIENTED_EDGE('',*,*,#1793,.F.);
#2698=ORIENTED_EDGE('',*,*,#1796,.F.);
#2699=ORIENTED_EDGE('',*,*,#1954,.F.);
#2700=ORIENTED_EDGE('',*,*,#1801,.F.);
#2701=ORIENTED_EDGE('',*,*,#1955,.F.);
#2702=ORIENTED_EDGE('',*,*,#1843,.T.);
#2703=ORIENTED_EDGE('',*,*,#1951,.T.);
#2704=ORIENTED_EDGE('',*,*,#1841,.T.);
#2705=ORIENTED_EDGE('',*,*,#1838,.T.);
#2706=ORIENTED_EDGE('',*,*,#1835,.T.);
#2707=ORIENTED_EDGE('',*,*,#1832,.T.);
#2708=ORIENTED_EDGE('',*,*,#1829,.T.);
#2709=ORIENTED_EDGE('',*,*,#1826,.T.);
#2710=ORIENTED_EDGE('',*,*,#1823,.T.);
#2711=ORIENTED_EDGE('',*,*,#1820,.T.);
#2712=ORIENTED_EDGE('',*,*,#1817,.T.);
#2713=ORIENTED_EDGE('',*,*,#1814,.T.);
#2714=ORIENTED_EDGE('',*,*,#1811,.T.);
#2715=ORIENTED_EDGE('',*,*,#1808,.T.);
#2716=ORIENTED_EDGE('',*,*,#1805,.T.);
#2717=ORIENTED_EDGE('',*,*,#1798,.T.);
#2718=ORIENTED_EDGE('',*,*,#1954,.T.);
#2719=ORIENTED_EDGE('',*,*,#1795,.F.);
#2720=ORIENTED_EDGE('',*,*,#1953,.T.);
#2721=ORIENTED_EDGE('',*,*,#1763,.F.);
#2722=ORIENTED_EDGE('',*,*,#1851,.F.);
#2723=ORIENTED_EDGE('',*,*,#1956,.T.);
#2724=ORIENTED_EDGE('',*,*,#1957,.T.);
#2725=ORIENTED_EDGE('',*,*,#1958,.F.);
#2726=ORIENTED_EDGE('',*,*,#1959,.F.);
#2727=ORIENTED_EDGE('',*,*,#1960,.T.);
#2728=ORIENTED_EDGE('',*,*,#1959,.T.);
#2729=ORIENTED_EDGE('',*,*,#1961,.F.);
#2730=ORIENTED_EDGE('',*,*,#1962,.F.);
#2731=ORIENTED_EDGE('',*,*,#1963,.T.);
#2732=ORIENTED_EDGE('',*,*,#1962,.T.);
#2733=ORIENTED_EDGE('',*,*,#1964,.F.);
#2734=ORIENTED_EDGE('',*,*,#1965,.F.);
#2735=ORIENTED_EDGE('',*,*,#1966,.T.);
#2736=ORIENTED_EDGE('',*,*,#1965,.T.);
#2737=ORIENTED_EDGE('',*,*,#1967,.F.);
#2738=ORIENTED_EDGE('',*,*,#1968,.F.);
#2739=ORIENTED_EDGE('',*,*,#1969,.T.);
#2740=ORIENTED_EDGE('',*,*,#1968,.T.);
#2741=ORIENTED_EDGE('',*,*,#1970,.F.);
#2742=ORIENTED_EDGE('',*,*,#1971,.F.);
#2743=ORIENTED_EDGE('',*,*,#1972,.T.);
#2744=ORIENTED_EDGE('',*,*,#1971,.T.);
#2745=ORIENTED_EDGE('',*,*,#1973,.F.);
#2746=ORIENTED_EDGE('',*,*,#1974,.F.);
#2747=ORIENTED_EDGE('',*,*,#1975,.T.);
#2748=ORIENTED_EDGE('',*,*,#1974,.T.);
#2749=ORIENTED_EDGE('',*,*,#1976,.F.);
#2750=ORIENTED_EDGE('',*,*,#1977,.F.);
#2751=ORIENTED_EDGE('',*,*,#1978,.T.);
#2752=ORIENTED_EDGE('',*,*,#1977,.T.);
#2753=ORIENTED_EDGE('',*,*,#1979,.F.);
#2754=ORIENTED_EDGE('',*,*,#1957,.F.);
#2755=ORIENTED_EDGE('',*,*,#1980,.F.);
#2756=ORIENTED_EDGE('',*,*,#1981,.T.);
#2757=ORIENTED_EDGE('',*,*,#1982,.F.);
#2758=ORIENTED_EDGE('',*,*,#1983,.F.);
#2759=ORIENTED_EDGE('',*,*,#1984,.T.);
#2760=ORIENTED_EDGE('',*,*,#1983,.T.);
#2761=ORIENTED_EDGE('',*,*,#1985,.F.);
#2762=ORIENTED_EDGE('',*,*,#1986,.F.);
#2763=ORIENTED_EDGE('',*,*,#1987,.F.);
#2764=ORIENTED_EDGE('',*,*,#1986,.T.);
#2765=ORIENTED_EDGE('',*,*,#1988,.F.);
#2766=ORIENTED_EDGE('',*,*,#1989,.F.);
#2767=ORIENTED_EDGE('',*,*,#1990,.T.);
#2768=ORIENTED_EDGE('',*,*,#1989,.T.);
#2769=ORIENTED_EDGE('',*,*,#1991,.F.);
#2770=ORIENTED_EDGE('',*,*,#1992,.F.);
#2771=ORIENTED_EDGE('',*,*,#1993,.T.);
#2772=ORIENTED_EDGE('',*,*,#1992,.T.);
#2773=ORIENTED_EDGE('',*,*,#1994,.F.);
#2774=ORIENTED_EDGE('',*,*,#1995,.F.);
#2775=ORIENTED_EDGE('',*,*,#1996,.T.);
#2776=ORIENTED_EDGE('',*,*,#1995,.T.);
#2777=ORIENTED_EDGE('',*,*,#1997,.F.);
#2778=ORIENTED_EDGE('',*,*,#1998,.F.);
#2779=ORIENTED_EDGE('',*,*,#1999,.T.);
#2780=ORIENTED_EDGE('',*,*,#1998,.T.);
#2781=ORIENTED_EDGE('',*,*,#2000,.F.);
#2782=ORIENTED_EDGE('',*,*,#2001,.F.);
#2783=ORIENTED_EDGE('',*,*,#2002,.T.);
#2784=ORIENTED_EDGE('',*,*,#2001,.T.);
#2785=ORIENTED_EDGE('',*,*,#2003,.F.);
#2786=ORIENTED_EDGE('',*,*,#2004,.F.);
#2787=ORIENTED_EDGE('',*,*,#2005,.F.);
#2788=ORIENTED_EDGE('',*,*,#2004,.T.);
#2789=ORIENTED_EDGE('',*,*,#2006,.F.);
#2790=ORIENTED_EDGE('',*,*,#2007,.F.);
#2791=ORIENTED_EDGE('',*,*,#2008,.T.);
#2792=ORIENTED_EDGE('',*,*,#2007,.T.);
#2793=ORIENTED_EDGE('',*,*,#2009,.F.);
#2794=ORIENTED_EDGE('',*,*,#2010,.F.);
#2795=ORIENTED_EDGE('',*,*,#2011,.F.);
#2796=ORIENTED_EDGE('',*,*,#2010,.T.);
#2797=ORIENTED_EDGE('',*,*,#2012,.F.);
#2798=ORIENTED_EDGE('',*,*,#2013,.F.);
#2799=ORIENTED_EDGE('',*,*,#2014,.T.);
#2800=ORIENTED_EDGE('',*,*,#2013,.T.);
#2801=ORIENTED_EDGE('',*,*,#2015,.F.);
#2802=ORIENTED_EDGE('',*,*,#2016,.F.);
#2803=ORIENTED_EDGE('',*,*,#2017,.T.);
#2804=ORIENTED_EDGE('',*,*,#2016,.T.);
#2805=ORIENTED_EDGE('',*,*,#2018,.F.);
#2806=ORIENTED_EDGE('',*,*,#2019,.F.);
#2807=ORIENTED_EDGE('',*,*,#2020,.T.);
#2808=ORIENTED_EDGE('',*,*,#2019,.T.);
#2809=ORIENTED_EDGE('',*,*,#2021,.F.);
#2810=ORIENTED_EDGE('',*,*,#2022,.F.);
#2811=ORIENTED_EDGE('',*,*,#1934,.T.);
#2812=ORIENTED_EDGE('',*,*,#1937,.T.);
#2813=ORIENTED_EDGE('',*,*,#1947,.T.);
#2814=ORIENTED_EDGE('',*,*,#1888,.T.);
#2815=ORIENTED_EDGE('',*,*,#1944,.T.);
#2816=ORIENTED_EDGE('',*,*,#1932,.T.);
#2817=ORIENTED_EDGE('',*,*,#1955,.T.);
#2818=ORIENTED_EDGE('',*,*,#1800,.T.);
#2819=ORIENTED_EDGE('',*,*,#1952,.T.);
#2820=ORIENTED_EDGE('',*,*,#1844,.T.);
#2821=ORIENTED_EDGE('',*,*,#2023,.T.);
#2822=ORIENTED_EDGE('',*,*,#2022,.T.);
#2823=ORIENTED_EDGE('',*,*,#2024,.F.);
#2824=ORIENTED_EDGE('',*,*,#2025,.F.);
#2825=ORIENTED_EDGE('',*,*,#2026,.T.);
#2826=ORIENTED_EDGE('',*,*,#2025,.T.);
#2827=ORIENTED_EDGE('',*,*,#2027,.F.);
#2828=ORIENTED_EDGE('',*,*,#1981,.F.);
#2829=ORIENTED_EDGE('',*,*,#2027,.T.);
#2830=ORIENTED_EDGE('',*,*,#2024,.T.);
#2831=ORIENTED_EDGE('',*,*,#2021,.T.);
#2832=ORIENTED_EDGE('',*,*,#2018,.T.);
#2833=ORIENTED_EDGE('',*,*,#2015,.T.);
#2834=ORIENTED_EDGE('',*,*,#2012,.T.);
#2835=ORIENTED_EDGE('',*,*,#2009,.T.);
#2836=ORIENTED_EDGE('',*,*,#2006,.T.);
#2837=ORIENTED_EDGE('',*,*,#2003,.T.);
#2838=ORIENTED_EDGE('',*,*,#2000,.T.);
#2839=ORIENTED_EDGE('',*,*,#1997,.T.);
#2840=ORIENTED_EDGE('',*,*,#1994,.T.);
#2841=ORIENTED_EDGE('',*,*,#1991,.T.);
#2842=ORIENTED_EDGE('',*,*,#1988,.T.);
#2843=ORIENTED_EDGE('',*,*,#1985,.T.);
#2844=ORIENTED_EDGE('',*,*,#1982,.T.);
#2845=ORIENTED_EDGE('',*,*,#1979,.T.);
#2846=ORIENTED_EDGE('',*,*,#1976,.T.);
#2847=ORIENTED_EDGE('',*,*,#1973,.T.);
#2848=ORIENTED_EDGE('',*,*,#1970,.T.);
#2849=ORIENTED_EDGE('',*,*,#1967,.T.);
#2850=ORIENTED_EDGE('',*,*,#1964,.T.);
#2851=ORIENTED_EDGE('',*,*,#1961,.T.);
#2852=ORIENTED_EDGE('',*,*,#1958,.T.);
#2853=ORIENTED_EDGE('',*,*,#2026,.F.);
#2854=ORIENTED_EDGE('',*,*,#1980,.T.);
#2855=ORIENTED_EDGE('',*,*,#1984,.F.);
#2856=ORIENTED_EDGE('',*,*,#1987,.T.);
#2857=ORIENTED_EDGE('',*,*,#1990,.F.);
#2858=ORIENTED_EDGE('',*,*,#1993,.F.);
#2859=ORIENTED_EDGE('',*,*,#1996,.F.);
#2860=ORIENTED_EDGE('',*,*,#1999,.F.);
#2861=ORIENTED_EDGE('',*,*,#2002,.F.);
#2862=ORIENTED_EDGE('',*,*,#2005,.T.);
#2863=ORIENTED_EDGE('',*,*,#2008,.F.);
#2864=ORIENTED_EDGE('',*,*,#2011,.T.);
#2865=ORIENTED_EDGE('',*,*,#2014,.F.);
#2866=ORIENTED_EDGE('',*,*,#2017,.F.);
#2867=ORIENTED_EDGE('',*,*,#2020,.F.);
#2868=ORIENTED_EDGE('',*,*,#2023,.F.);
#2869=ORIENTED_EDGE('',*,*,#1978,.F.);
#2870=ORIENTED_EDGE('',*,*,#1956,.F.);
#2871=ORIENTED_EDGE('',*,*,#1960,.F.);
#2872=ORIENTED_EDGE('',*,*,#1963,.F.);
#2873=ORIENTED_EDGE('',*,*,#1966,.F.);
#2874=ORIENTED_EDGE('',*,*,#1969,.F.);
#2875=ORIENTED_EDGE('',*,*,#1972,.F.);
#2876=ORIENTED_EDGE('',*,*,#1975,.F.);
#2877=ORIENTED_EDGE('',*,*,#2028,.T.);
#2878=ORIENTED_EDGE('',*,*,#2029,.T.);
#2879=ORIENTED_EDGE('',*,*,#2030,.F.);
#2880=ORIENTED_EDGE('',*,*,#2031,.F.);
#2881=ORIENTED_EDGE('',*,*,#2032,.T.);
#2882=ORIENTED_EDGE('',*,*,#2031,.T.);
#2883=ORIENTED_EDGE('',*,*,#2033,.F.);
#2884=ORIENTED_EDGE('',*,*,#2034,.F.);
#2885=ORIENTED_EDGE('',*,*,#2035,.T.);
#2886=ORIENTED_EDGE('',*,*,#2034,.T.);
#2887=ORIENTED_EDGE('',*,*,#2036,.F.);
#2888=ORIENTED_EDGE('',*,*,#2037,.F.);
#2889=ORIENTED_EDGE('',*,*,#2038,.T.);
#2890=ORIENTED_EDGE('',*,*,#2037,.T.);
#2891=ORIENTED_EDGE('',*,*,#2039,.F.);
#2892=ORIENTED_EDGE('',*,*,#2029,.F.);
#2893=ORIENTED_EDGE('',*,*,#2039,.T.);
#2894=ORIENTED_EDGE('',*,*,#2036,.T.);
#2895=ORIENTED_EDGE('',*,*,#2033,.T.);
#2896=ORIENTED_EDGE('',*,*,#2030,.T.);
#2897=ORIENTED_EDGE('',*,*,#2038,.F.);
#2898=ORIENTED_EDGE('',*,*,#2028,.F.);
#2899=ORIENTED_EDGE('',*,*,#2032,.F.);
#2900=ORIENTED_EDGE('',*,*,#2035,.F.);
#2901=ORIENTED_EDGE('',*,*,#2040,.F.);
#2902=ORIENTED_EDGE('',*,*,#2041,.T.);
#2903=ORIENTED_EDGE('',*,*,#2042,.T.);
#2904=ORIENTED_EDGE('',*,*,#2041,.F.);
#2905=ORIENTED_EDGE('',*,*,#2043,.F.);
#2906=ORIENTED_EDGE('',*,*,#2044,.T.);
#2907=ORIENTED_EDGE('',*,*,#2045,.T.);
#2908=ORIENTED_EDGE('',*,*,#2044,.F.);
#2909=ORIENTED_EDGE('',*,*,#2043,.T.);
#2910=ORIENTED_EDGE('',*,*,#2040,.T.);
#2911=ORIENTED_EDGE('',*,*,#2045,.F.);
#2912=ORIENTED_EDGE('',*,*,#2042,.F.);
#2913=ORIENTED_EDGE('',*,*,#2046,.F.);
#2914=ORIENTED_EDGE('',*,*,#2047,.T.);
#2915=ORIENTED_EDGE('',*,*,#2048,.T.);
#2916=ORIENTED_EDGE('',*,*,#2049,.T.);
#2917=ORIENTED_EDGE('',*,*,#2050,.F.);
#2918=ORIENTED_EDGE('',*,*,#2051,.T.);
#2919=ORIENTED_EDGE('',*,*,#2046,.T.);
#2920=ORIENTED_EDGE('',*,*,#2052,.T.);
#2921=ORIENTED_EDGE('',*,*,#2053,.F.);
#2922=ORIENTED_EDGE('',*,*,#2054,.T.);
#2923=ORIENTED_EDGE('',*,*,#2050,.T.);
#2924=ORIENTED_EDGE('',*,*,#2055,.T.);
#2925=ORIENTED_EDGE('',*,*,#2056,.F.);
#2926=ORIENTED_EDGE('',*,*,#2057,.T.);
#2927=ORIENTED_EDGE('',*,*,#2053,.T.);
#2928=ORIENTED_EDGE('',*,*,#2058,.T.);
#2929=ORIENTED_EDGE('',*,*,#2059,.F.);
#2930=ORIENTED_EDGE('',*,*,#2060,.T.);
#2931=ORIENTED_EDGE('',*,*,#2056,.T.);
#2932=ORIENTED_EDGE('',*,*,#2061,.T.);
#2933=ORIENTED_EDGE('',*,*,#2062,.F.);
#2934=ORIENTED_EDGE('',*,*,#2063,.T.);
#2935=ORIENTED_EDGE('',*,*,#2059,.T.);
#2936=ORIENTED_EDGE('',*,*,#2064,.T.);
#2937=ORIENTED_EDGE('',*,*,#2065,.F.);
#2938=ORIENTED_EDGE('',*,*,#2066,.T.);
#2939=ORIENTED_EDGE('',*,*,#2062,.T.);
#2940=ORIENTED_EDGE('',*,*,#2067,.T.);
#2941=ORIENTED_EDGE('',*,*,#2068,.F.);
#2942=ORIENTED_EDGE('',*,*,#2069,.T.);
#2943=ORIENTED_EDGE('',*,*,#2065,.T.);
#2944=ORIENTED_EDGE('',*,*,#2070,.T.);
#2945=ORIENTED_EDGE('',*,*,#2071,.F.);
#2946=ORIENTED_EDGE('',*,*,#2072,.T.);
#2947=ORIENTED_EDGE('',*,*,#2068,.T.);
#2948=ORIENTED_EDGE('',*,*,#2073,.T.);
#2949=ORIENTED_EDGE('',*,*,#2074,.F.);
#2950=ORIENTED_EDGE('',*,*,#2075,.T.);
#2951=ORIENTED_EDGE('',*,*,#2071,.T.);
#2952=ORIENTED_EDGE('',*,*,#2076,.T.);
#2953=ORIENTED_EDGE('',*,*,#2077,.F.);
#2954=ORIENTED_EDGE('',*,*,#2078,.T.);
#2955=ORIENTED_EDGE('',*,*,#2074,.T.);
#2956=ORIENTED_EDGE('',*,*,#2079,.T.);
#2957=ORIENTED_EDGE('',*,*,#2080,.F.);
#2958=ORIENTED_EDGE('',*,*,#2081,.T.);
#2959=ORIENTED_EDGE('',*,*,#2077,.T.);
#2960=ORIENTED_EDGE('',*,*,#2082,.T.);
#2961=ORIENTED_EDGE('',*,*,#2083,.F.);
#2962=ORIENTED_EDGE('',*,*,#2084,.T.);
#2963=ORIENTED_EDGE('',*,*,#2080,.T.);
#2964=ORIENTED_EDGE('',*,*,#2085,.T.);
#2965=ORIENTED_EDGE('',*,*,#2086,.F.);
#2966=ORIENTED_EDGE('',*,*,#2087,.T.);
#2967=ORIENTED_EDGE('',*,*,#2083,.T.);
#2968=ORIENTED_EDGE('',*,*,#2088,.T.);
#2969=ORIENTED_EDGE('',*,*,#2089,.F.);
#2970=ORIENTED_EDGE('',*,*,#2090,.T.);
#2971=ORIENTED_EDGE('',*,*,#2086,.T.);
#2972=ORIENTED_EDGE('',*,*,#2091,.T.);
#2973=ORIENTED_EDGE('',*,*,#2092,.F.);
#2974=ORIENTED_EDGE('',*,*,#2093,.T.);
#2975=ORIENTED_EDGE('',*,*,#2089,.T.);
#2976=ORIENTED_EDGE('',*,*,#2094,.T.);
#2977=ORIENTED_EDGE('',*,*,#2095,.F.);
#2978=ORIENTED_EDGE('',*,*,#2096,.T.);
#2979=ORIENTED_EDGE('',*,*,#2092,.T.);
#2980=ORIENTED_EDGE('',*,*,#2097,.T.);
#2981=ORIENTED_EDGE('',*,*,#2098,.F.);
#2982=ORIENTED_EDGE('',*,*,#2099,.T.);
#2983=ORIENTED_EDGE('',*,*,#2095,.T.);
#2984=ORIENTED_EDGE('',*,*,#2100,.T.);
#2985=ORIENTED_EDGE('',*,*,#2101,.F.);
#2986=ORIENTED_EDGE('',*,*,#2102,.T.);
#2987=ORIENTED_EDGE('',*,*,#2098,.T.);
#2988=ORIENTED_EDGE('',*,*,#2103,.T.);
#2989=ORIENTED_EDGE('',*,*,#2104,.F.);
#2990=ORIENTED_EDGE('',*,*,#2105,.T.);
#2991=ORIENTED_EDGE('',*,*,#2101,.T.);
#2992=ORIENTED_EDGE('',*,*,#2106,.T.);
#2993=ORIENTED_EDGE('',*,*,#2107,.F.);
#2994=ORIENTED_EDGE('',*,*,#2108,.T.);
#2995=ORIENTED_EDGE('',*,*,#2104,.T.);
#2996=ORIENTED_EDGE('',*,*,#2109,.T.);
#2997=ORIENTED_EDGE('',*,*,#2110,.F.);
#2998=ORIENTED_EDGE('',*,*,#2111,.T.);
#2999=ORIENTED_EDGE('',*,*,#2107,.T.);
#3000=ORIENTED_EDGE('',*,*,#2112,.T.);
#3001=ORIENTED_EDGE('',*,*,#2113,.F.);
#3002=ORIENTED_EDGE('',*,*,#2114,.T.);
#3003=ORIENTED_EDGE('',*,*,#2110,.T.);
#3004=ORIENTED_EDGE('',*,*,#2115,.T.);
#3005=ORIENTED_EDGE('',*,*,#2116,.F.);
#3006=ORIENTED_EDGE('',*,*,#2117,.T.);
#3007=ORIENTED_EDGE('',*,*,#2113,.T.);
#3008=ORIENTED_EDGE('',*,*,#2118,.T.);
#3009=ORIENTED_EDGE('',*,*,#2119,.F.);
#3010=ORIENTED_EDGE('',*,*,#2120,.T.);
#3011=ORIENTED_EDGE('',*,*,#2116,.T.);
#3012=ORIENTED_EDGE('',*,*,#2121,.T.);
#3013=ORIENTED_EDGE('',*,*,#2122,.F.);
#3014=ORIENTED_EDGE('',*,*,#2123,.T.);
#3015=ORIENTED_EDGE('',*,*,#2119,.T.);
#3016=ORIENTED_EDGE('',*,*,#2124,.T.);
#3017=ORIENTED_EDGE('',*,*,#2125,.F.);
#3018=ORIENTED_EDGE('',*,*,#2126,.T.);
#3019=ORIENTED_EDGE('',*,*,#2122,.T.);
#3020=ORIENTED_EDGE('',*,*,#2127,.T.);
#3021=ORIENTED_EDGE('',*,*,#2128,.F.);
#3022=ORIENTED_EDGE('',*,*,#2129,.T.);
#3023=ORIENTED_EDGE('',*,*,#2125,.T.);
#3024=ORIENTED_EDGE('',*,*,#2130,.T.);
#3025=ORIENTED_EDGE('',*,*,#2131,.F.);
#3026=ORIENTED_EDGE('',*,*,#2132,.T.);
#3027=ORIENTED_EDGE('',*,*,#2128,.T.);
#3028=ORIENTED_EDGE('',*,*,#2133,.T.);
#3029=ORIENTED_EDGE('',*,*,#2134,.F.);
#3030=ORIENTED_EDGE('',*,*,#2135,.T.);
#3031=ORIENTED_EDGE('',*,*,#2131,.T.);
#3032=ORIENTED_EDGE('',*,*,#2136,.T.);
#3033=ORIENTED_EDGE('',*,*,#2137,.F.);
#3034=ORIENTED_EDGE('',*,*,#2138,.T.);
#3035=ORIENTED_EDGE('',*,*,#2139,.T.);
#3036=ORIENTED_EDGE('',*,*,#2140,.F.);
#3037=ORIENTED_EDGE('',*,*,#2141,.F.);
#3038=ORIENTED_EDGE('',*,*,#2142,.T.);
#3039=ORIENTED_EDGE('',*,*,#2137,.T.);
#3040=ORIENTED_EDGE('',*,*,#2143,.F.);
#3041=ORIENTED_EDGE('',*,*,#2144,.F.);
#3042=ORIENTED_EDGE('',*,*,#2145,.T.);
#3043=ORIENTED_EDGE('',*,*,#2141,.T.);
#3044=ORIENTED_EDGE('',*,*,#2146,.F.);
#3045=ORIENTED_EDGE('',*,*,#2147,.F.);
#3046=ORIENTED_EDGE('',*,*,#2148,.T.);
#3047=ORIENTED_EDGE('',*,*,#2144,.T.);
#3048=ORIENTED_EDGE('',*,*,#2149,.F.);
#3049=ORIENTED_EDGE('',*,*,#2150,.F.);
#3050=ORIENTED_EDGE('',*,*,#2151,.T.);
#3051=ORIENTED_EDGE('',*,*,#2147,.T.);
#3052=ORIENTED_EDGE('',*,*,#2152,.F.);
#3053=ORIENTED_EDGE('',*,*,#2153,.F.);
#3054=ORIENTED_EDGE('',*,*,#2154,.T.);
#3055=ORIENTED_EDGE('',*,*,#2150,.T.);
#3056=ORIENTED_EDGE('',*,*,#2155,.F.);
#3057=ORIENTED_EDGE('',*,*,#2156,.F.);
#3058=ORIENTED_EDGE('',*,*,#2157,.T.);
#3059=ORIENTED_EDGE('',*,*,#2153,.T.);
#3060=ORIENTED_EDGE('',*,*,#2158,.F.);
#3061=ORIENTED_EDGE('',*,*,#2159,.F.);
#3062=ORIENTED_EDGE('',*,*,#2160,.T.);
#3063=ORIENTED_EDGE('',*,*,#2156,.T.);
#3064=ORIENTED_EDGE('',*,*,#2161,.F.);
#3065=ORIENTED_EDGE('',*,*,#2162,.F.);
#3066=ORIENTED_EDGE('',*,*,#2163,.T.);
#3067=ORIENTED_EDGE('',*,*,#2159,.T.);
#3068=ORIENTED_EDGE('',*,*,#2164,.F.);
#3069=ORIENTED_EDGE('',*,*,#2165,.F.);
#3070=ORIENTED_EDGE('',*,*,#2166,.T.);
#3071=ORIENTED_EDGE('',*,*,#2162,.T.);
#3072=ORIENTED_EDGE('',*,*,#2167,.F.);
#3073=ORIENTED_EDGE('',*,*,#2168,.F.);
#3074=ORIENTED_EDGE('',*,*,#2169,.T.);
#3075=ORIENTED_EDGE('',*,*,#2165,.T.);
#3076=ORIENTED_EDGE('',*,*,#2170,.F.);
#3077=ORIENTED_EDGE('',*,*,#2171,.F.);
#3078=ORIENTED_EDGE('',*,*,#2172,.T.);
#3079=ORIENTED_EDGE('',*,*,#2168,.T.);
#3080=ORIENTED_EDGE('',*,*,#2173,.F.);
#3081=ORIENTED_EDGE('',*,*,#2174,.F.);
#3082=ORIENTED_EDGE('',*,*,#2175,.T.);
#3083=ORIENTED_EDGE('',*,*,#2171,.T.);
#3084=ORIENTED_EDGE('',*,*,#2176,.F.);
#3085=ORIENTED_EDGE('',*,*,#2177,.F.);
#3086=ORIENTED_EDGE('',*,*,#2178,.T.);
#3087=ORIENTED_EDGE('',*,*,#2174,.T.);
#3088=ORIENTED_EDGE('',*,*,#2179,.F.);
#3089=ORIENTED_EDGE('',*,*,#2180,.F.);
#3090=ORIENTED_EDGE('',*,*,#2181,.T.);
#3091=ORIENTED_EDGE('',*,*,#2177,.T.);
#3092=ORIENTED_EDGE('',*,*,#2182,.F.);
#3093=ORIENTED_EDGE('',*,*,#2183,.F.);
#3094=ORIENTED_EDGE('',*,*,#2184,.T.);
#3095=ORIENTED_EDGE('',*,*,#2180,.T.);
#3096=ORIENTED_EDGE('',*,*,#2185,.F.);
#3097=ORIENTED_EDGE('',*,*,#2186,.F.);
#3098=ORIENTED_EDGE('',*,*,#2187,.T.);
#3099=ORIENTED_EDGE('',*,*,#2183,.T.);
#3100=ORIENTED_EDGE('',*,*,#2188,.F.);
#3101=ORIENTED_EDGE('',*,*,#2189,.F.);
#3102=ORIENTED_EDGE('',*,*,#2190,.T.);
#3103=ORIENTED_EDGE('',*,*,#2186,.T.);
#3104=ORIENTED_EDGE('',*,*,#2191,.F.);
#3105=ORIENTED_EDGE('',*,*,#2192,.F.);
#3106=ORIENTED_EDGE('',*,*,#2193,.T.);
#3107=ORIENTED_EDGE('',*,*,#2189,.T.);
#3108=ORIENTED_EDGE('',*,*,#2194,.F.);
#3109=ORIENTED_EDGE('',*,*,#2195,.F.);
#3110=ORIENTED_EDGE('',*,*,#2196,.T.);
#3111=ORIENTED_EDGE('',*,*,#2192,.T.);
#3112=ORIENTED_EDGE('',*,*,#2197,.F.);
#3113=ORIENTED_EDGE('',*,*,#2198,.F.);
#3114=ORIENTED_EDGE('',*,*,#2199,.T.);
#3115=ORIENTED_EDGE('',*,*,#2195,.T.);
#3116=ORIENTED_EDGE('',*,*,#2200,.F.);
#3117=ORIENTED_EDGE('',*,*,#2201,.F.);
#3118=ORIENTED_EDGE('',*,*,#2202,.T.);
#3119=ORIENTED_EDGE('',*,*,#2198,.T.);
#3120=ORIENTED_EDGE('',*,*,#2203,.F.);
#3121=ORIENTED_EDGE('',*,*,#2204,.F.);
#3122=ORIENTED_EDGE('',*,*,#2205,.T.);
#3123=ORIENTED_EDGE('',*,*,#2201,.T.);
#3124=ORIENTED_EDGE('',*,*,#2206,.F.);
#3125=ORIENTED_EDGE('',*,*,#2207,.F.);
#3126=ORIENTED_EDGE('',*,*,#2208,.T.);
#3127=ORIENTED_EDGE('',*,*,#2204,.T.);
#3128=ORIENTED_EDGE('',*,*,#2209,.F.);
#3129=ORIENTED_EDGE('',*,*,#2210,.F.);
#3130=ORIENTED_EDGE('',*,*,#2211,.T.);
#3131=ORIENTED_EDGE('',*,*,#2207,.T.);
#3132=ORIENTED_EDGE('',*,*,#2212,.F.);
#3133=ORIENTED_EDGE('',*,*,#2213,.F.);
#3134=ORIENTED_EDGE('',*,*,#2214,.T.);
#3135=ORIENTED_EDGE('',*,*,#2210,.T.);
#3136=ORIENTED_EDGE('',*,*,#2215,.F.);
#3137=ORIENTED_EDGE('',*,*,#2216,.F.);
#3138=ORIENTED_EDGE('',*,*,#2217,.T.);
#3139=ORIENTED_EDGE('',*,*,#2213,.T.);
#3140=ORIENTED_EDGE('',*,*,#2218,.F.);
#3141=ORIENTED_EDGE('',*,*,#2219,.F.);
#3142=ORIENTED_EDGE('',*,*,#2220,.T.);
#3143=ORIENTED_EDGE('',*,*,#2216,.T.);
#3144=ORIENTED_EDGE('',*,*,#2221,.F.);
#3145=ORIENTED_EDGE('',*,*,#2222,.F.);
#3146=ORIENTED_EDGE('',*,*,#2223,.T.);
#3147=ORIENTED_EDGE('',*,*,#2219,.T.);
#3148=ORIENTED_EDGE('',*,*,#2224,.F.);
#3149=ORIENTED_EDGE('',*,*,#2225,.F.);
#3150=ORIENTED_EDGE('',*,*,#2226,.T.);
#3151=ORIENTED_EDGE('',*,*,#2222,.T.);
#3152=ORIENTED_EDGE('',*,*,#2227,.F.);
#3153=ORIENTED_EDGE('',*,*,#2228,.F.);
#3154=ORIENTED_EDGE('',*,*,#2139,.F.);
#3155=ORIENTED_EDGE('',*,*,#2229,.F.);
#3156=ORIENTED_EDGE('',*,*,#2230,.F.);
#3157=ORIENTED_EDGE('',*,*,#2231,.F.);
#3158=ORIENTED_EDGE('',*,*,#2232,.T.);
#3159=ORIENTED_EDGE('',*,*,#2233,.F.);
#3160=ORIENTED_EDGE('',*,*,#2232,.F.);
#3161=ORIENTED_EDGE('',*,*,#2229,.T.);
#3162=ORIENTED_EDGE('',*,*,#2138,.F.);
#3163=ORIENTED_EDGE('',*,*,#2142,.F.);
#3164=ORIENTED_EDGE('',*,*,#2145,.F.);
#3165=ORIENTED_EDGE('',*,*,#2148,.F.);
#3166=ORIENTED_EDGE('',*,*,#2151,.F.);
#3167=ORIENTED_EDGE('',*,*,#2154,.F.);
#3168=ORIENTED_EDGE('',*,*,#2157,.F.);
#3169=ORIENTED_EDGE('',*,*,#2160,.F.);
#3170=ORIENTED_EDGE('',*,*,#2163,.F.);
#3171=ORIENTED_EDGE('',*,*,#2166,.F.);
#3172=ORIENTED_EDGE('',*,*,#2169,.F.);
#3173=ORIENTED_EDGE('',*,*,#2172,.F.);
#3174=ORIENTED_EDGE('',*,*,#2175,.F.);
#3175=ORIENTED_EDGE('',*,*,#2178,.F.);
#3176=ORIENTED_EDGE('',*,*,#2181,.F.);
#3177=ORIENTED_EDGE('',*,*,#2184,.F.);
#3178=ORIENTED_EDGE('',*,*,#2187,.F.);
#3179=ORIENTED_EDGE('',*,*,#2190,.F.);
#3180=ORIENTED_EDGE('',*,*,#2193,.F.);
#3181=ORIENTED_EDGE('',*,*,#2196,.F.);
#3182=ORIENTED_EDGE('',*,*,#2199,.F.);
#3183=ORIENTED_EDGE('',*,*,#2202,.F.);
#3184=ORIENTED_EDGE('',*,*,#2205,.F.);
#3185=ORIENTED_EDGE('',*,*,#2208,.F.);
#3186=ORIENTED_EDGE('',*,*,#2211,.F.);
#3187=ORIENTED_EDGE('',*,*,#2214,.F.);
#3188=ORIENTED_EDGE('',*,*,#2217,.F.);
#3189=ORIENTED_EDGE('',*,*,#2220,.F.);
#3190=ORIENTED_EDGE('',*,*,#2223,.F.);
#3191=ORIENTED_EDGE('',*,*,#2226,.F.);
#3192=ORIENTED_EDGE('',*,*,#2234,.F.);
#3193=ORIENTED_EDGE('',*,*,#2235,.F.);
#3194=ORIENTED_EDGE('',*,*,#2047,.F.);
#3195=ORIENTED_EDGE('',*,*,#2051,.F.);
#3196=ORIENTED_EDGE('',*,*,#2054,.F.);
#3197=ORIENTED_EDGE('',*,*,#2057,.F.);
#3198=ORIENTED_EDGE('',*,*,#2060,.F.);
#3199=ORIENTED_EDGE('',*,*,#2063,.F.);
#3200=ORIENTED_EDGE('',*,*,#2066,.F.);
#3201=ORIENTED_EDGE('',*,*,#2069,.F.);
#3202=ORIENTED_EDGE('',*,*,#2072,.F.);
#3203=ORIENTED_EDGE('',*,*,#2075,.F.);
#3204=ORIENTED_EDGE('',*,*,#2078,.F.);
#3205=ORIENTED_EDGE('',*,*,#2081,.F.);
#3206=ORIENTED_EDGE('',*,*,#2084,.F.);
#3207=ORIENTED_EDGE('',*,*,#2087,.F.);
#3208=ORIENTED_EDGE('',*,*,#2090,.F.);
#3209=ORIENTED_EDGE('',*,*,#2093,.F.);
#3210=ORIENTED_EDGE('',*,*,#2096,.F.);
#3211=ORIENTED_EDGE('',*,*,#2099,.F.);
#3212=ORIENTED_EDGE('',*,*,#2102,.F.);
#3213=ORIENTED_EDGE('',*,*,#2105,.F.);
#3214=ORIENTED_EDGE('',*,*,#2108,.F.);
#3215=ORIENTED_EDGE('',*,*,#2111,.F.);
#3216=ORIENTED_EDGE('',*,*,#2114,.F.);
#3217=ORIENTED_EDGE('',*,*,#2117,.F.);
#3218=ORIENTED_EDGE('',*,*,#2120,.F.);
#3219=ORIENTED_EDGE('',*,*,#2123,.F.);
#3220=ORIENTED_EDGE('',*,*,#2126,.F.);
#3221=ORIENTED_EDGE('',*,*,#2129,.F.);
#3222=ORIENTED_EDGE('',*,*,#2132,.F.);
#3223=ORIENTED_EDGE('',*,*,#2135,.F.);
#3224=ORIENTED_EDGE('',*,*,#2236,.F.);
#3225=ORIENTED_EDGE('',*,*,#2225,.T.);
#3226=ORIENTED_EDGE('',*,*,#2237,.F.);
#3227=ORIENTED_EDGE('',*,*,#2238,.F.);
#3228=ORIENTED_EDGE('',*,*,#2234,.T.);
#3229=ORIENTED_EDGE('',*,*,#2228,.T.);
#3230=ORIENTED_EDGE('',*,*,#2231,.T.);
#3231=ORIENTED_EDGE('',*,*,#2239,.F.);
#3232=ORIENTED_EDGE('',*,*,#2136,.F.);
#3233=ORIENTED_EDGE('',*,*,#2133,.F.);
#3234=ORIENTED_EDGE('',*,*,#2130,.F.);
#3235=ORIENTED_EDGE('',*,*,#2127,.F.);
#3236=ORIENTED_EDGE('',*,*,#2124,.F.);
#3237=ORIENTED_EDGE('',*,*,#2121,.F.);
#3238=ORIENTED_EDGE('',*,*,#2118,.F.);
#3239=ORIENTED_EDGE('',*,*,#2115,.F.);
#3240=ORIENTED_EDGE('',*,*,#2112,.F.);
#3241=ORIENTED_EDGE('',*,*,#2109,.F.);
#3242=ORIENTED_EDGE('',*,*,#2106,.F.);
#3243=ORIENTED_EDGE('',*,*,#2103,.F.);
#3244=ORIENTED_EDGE('',*,*,#2100,.F.);
#3245=ORIENTED_EDGE('',*,*,#2097,.F.);
#3246=ORIENTED_EDGE('',*,*,#2094,.F.);
#3247=ORIENTED_EDGE('',*,*,#2091,.F.);
#3248=ORIENTED_EDGE('',*,*,#2088,.F.);
#3249=ORIENTED_EDGE('',*,*,#2085,.F.);
#3250=ORIENTED_EDGE('',*,*,#2082,.F.);
#3251=ORIENTED_EDGE('',*,*,#2079,.F.);
#3252=ORIENTED_EDGE('',*,*,#2076,.F.);
#3253=ORIENTED_EDGE('',*,*,#2073,.F.);
#3254=ORIENTED_EDGE('',*,*,#2070,.F.);
#3255=ORIENTED_EDGE('',*,*,#2067,.F.);
#3256=ORIENTED_EDGE('',*,*,#2064,.F.);
#3257=ORIENTED_EDGE('',*,*,#2061,.F.);
#3258=ORIENTED_EDGE('',*,*,#2058,.F.);
#3259=ORIENTED_EDGE('',*,*,#2055,.F.);
#3260=ORIENTED_EDGE('',*,*,#2052,.F.);
#3261=ORIENTED_EDGE('',*,*,#2049,.F.);
#3262=ORIENTED_EDGE('',*,*,#2240,.F.);
#3263=ORIENTED_EDGE('',*,*,#2237,.T.);
#3264=ORIENTED_EDGE('',*,*,#2227,.T.);
#3265=ORIENTED_EDGE('',*,*,#2224,.T.);
#3266=ORIENTED_EDGE('',*,*,#2221,.T.);
#3267=ORIENTED_EDGE('',*,*,#2218,.T.);
#3268=ORIENTED_EDGE('',*,*,#2215,.T.);
#3269=ORIENTED_EDGE('',*,*,#2212,.T.);
#3270=ORIENTED_EDGE('',*,*,#2209,.T.);
#3271=ORIENTED_EDGE('',*,*,#2206,.T.);
#3272=ORIENTED_EDGE('',*,*,#2203,.T.);
#3273=ORIENTED_EDGE('',*,*,#2200,.T.);
#3274=ORIENTED_EDGE('',*,*,#2197,.T.);
#3275=ORIENTED_EDGE('',*,*,#2194,.T.);
#3276=ORIENTED_EDGE('',*,*,#2191,.T.);
#3277=ORIENTED_EDGE('',*,*,#2188,.T.);
#3278=ORIENTED_EDGE('',*,*,#2185,.T.);
#3279=ORIENTED_EDGE('',*,*,#2182,.T.);
#3280=ORIENTED_EDGE('',*,*,#2179,.T.);
#3281=ORIENTED_EDGE('',*,*,#2176,.T.);
#3282=ORIENTED_EDGE('',*,*,#2173,.T.);
#3283=ORIENTED_EDGE('',*,*,#2170,.T.);
#3284=ORIENTED_EDGE('',*,*,#2167,.T.);
#3285=ORIENTED_EDGE('',*,*,#2164,.T.);
#3286=ORIENTED_EDGE('',*,*,#2161,.T.);
#3287=ORIENTED_EDGE('',*,*,#2158,.T.);
#3288=ORIENTED_EDGE('',*,*,#2155,.T.);
#3289=ORIENTED_EDGE('',*,*,#2152,.T.);
#3290=ORIENTED_EDGE('',*,*,#2149,.T.);
#3291=ORIENTED_EDGE('',*,*,#2146,.T.);
#3292=ORIENTED_EDGE('',*,*,#2143,.T.);
#3293=ORIENTED_EDGE('',*,*,#2140,.T.);
#3294=ORIENTED_EDGE('',*,*,#2134,.T.);
#3295=ORIENTED_EDGE('',*,*,#2239,.T.);
#3296=ORIENTED_EDGE('',*,*,#2230,.T.);
#3297=ORIENTED_EDGE('',*,*,#2236,.T.);
#3298=ORIENTED_EDGE('',*,*,#2241,.F.);
#3299=ORIENTED_EDGE('',*,*,#2242,.T.);
#3300=ORIENTED_EDGE('',*,*,#2243,.T.);
#3301=ORIENTED_EDGE('',*,*,#2244,.F.);
#3302=ORIENTED_EDGE('',*,*,#2245,.F.);
#3303=ORIENTED_EDGE('',*,*,#2246,.T.);
#3304=ORIENTED_EDGE('',*,*,#2247,.T.);
#3305=ORIENTED_EDGE('',*,*,#2242,.F.);
#3306=ORIENTED_EDGE('',*,*,#2248,.F.);
#3307=ORIENTED_EDGE('',*,*,#2249,.T.);
#3308=ORIENTED_EDGE('',*,*,#2250,.T.);
#3309=ORIENTED_EDGE('',*,*,#2246,.F.);
#3310=ORIENTED_EDGE('',*,*,#2251,.F.);
#3311=ORIENTED_EDGE('',*,*,#2252,.T.);
#3312=ORIENTED_EDGE('',*,*,#2253,.T.);
#3313=ORIENTED_EDGE('',*,*,#2249,.F.);
#3314=ORIENTED_EDGE('',*,*,#2254,.F.);
#3315=ORIENTED_EDGE('',*,*,#2255,.T.);
#3316=ORIENTED_EDGE('',*,*,#2256,.T.);
#3317=ORIENTED_EDGE('',*,*,#2252,.F.);
#3318=ORIENTED_EDGE('',*,*,#2257,.F.);
#3319=ORIENTED_EDGE('',*,*,#2244,.T.);
#3320=ORIENTED_EDGE('',*,*,#2258,.T.);
#3321=ORIENTED_EDGE('',*,*,#2255,.F.);
#3322=ORIENTED_EDGE('',*,*,#2258,.F.);
#3323=ORIENTED_EDGE('',*,*,#2243,.F.);
#3324=ORIENTED_EDGE('',*,*,#2247,.F.);
#3325=ORIENTED_EDGE('',*,*,#2250,.F.);
#3326=ORIENTED_EDGE('',*,*,#2253,.F.);
#3327=ORIENTED_EDGE('',*,*,#2256,.F.);
#3328=ORIENTED_EDGE('',*,*,#2259,.T.);
#3329=ORIENTED_EDGE('',*,*,#2235,.T.);
#3330=ORIENTED_EDGE('',*,*,#2238,.T.);
#3331=ORIENTED_EDGE('',*,*,#2240,.T.);
#3332=ORIENTED_EDGE('',*,*,#2048,.F.);
#3333=ORIENTED_EDGE('',*,*,#2259,.F.);
#3334=ORIENTED_EDGE('',*,*,#2260,.T.);
#3335=ORIENTED_EDGE('',*,*,#2261,.T.);
#3336=ORIENTED_EDGE('',*,*,#2260,.F.);
#3337=ORIENTED_EDGE('',*,*,#2261,.F.);
#3338=ORIENTED_EDGE('',*,*,#2241,.T.);
#3339=ORIENTED_EDGE('',*,*,#2257,.T.);
#3340=ORIENTED_EDGE('',*,*,#2254,.T.);
#3341=ORIENTED_EDGE('',*,*,#2251,.T.);
#3342=ORIENTED_EDGE('',*,*,#2248,.T.);
#3343=ORIENTED_EDGE('',*,*,#2245,.T.);
#3344=ORIENTED_EDGE('',*,*,#2233,.T.);
#3345=ORIENTED_EDGE('',*,*,#2262,.F.);
#3346=ORIENTED_EDGE('',*,*,#2263,.T.);
#3347=ORIENTED_EDGE('',*,*,#2264,.T.);
#3348=ORIENTED_EDGE('',*,*,#2263,.F.);
#3349=ORIENTED_EDGE('',*,*,#2262,.T.);
#3350=ORIENTED_EDGE('',*,*,#2264,.F.);
#3351=CYLINDRICAL_SURFACE('',#3770,1.);
#3352=CYLINDRICAL_SURFACE('',#3774,1.);
#3353=CYLINDRICAL_SURFACE('',#3778,3.5);
#3354=CYLINDRICAL_SURFACE('',#3781,3.5);
#3355=CYLINDRICAL_SURFACE('',#3784,3.5);
#3356=CYLINDRICAL_SURFACE('',#3787,3.5);
#3357=CYLINDRICAL_SURFACE('',#3790,3.);
#3358=CYLINDRICAL_SURFACE('',#3793,3.);
#3359=CYLINDRICAL_SURFACE('',#3803,2.117);
#3360=CYLINDRICAL_SURFACE('',#3806,2.117);
#3361=CYLINDRICAL_SURFACE('',#3807,2.117);
#3362=CYLINDRICAL_SURFACE('',#3808,2.117);
#3363=CYLINDRICAL_SURFACE('',#3809,2.117);
#3364=CYLINDRICAL_SURFACE('',#3810,2.117);
#3365=CYLINDRICAL_SURFACE('',#3811,2.117);
#3366=CYLINDRICAL_SURFACE('',#3812,2.117);
#3367=CYLINDRICAL_SURFACE('',#3813,2.117);
#3368=CYLINDRICAL_SURFACE('',#3814,2.117);
#3369=CYLINDRICAL_SURFACE('',#3815,2.117);
#3370=CYLINDRICAL_SURFACE('',#3816,2.117);
#3371=CYLINDRICAL_SURFACE('',#3817,2.117);
#3372=CYLINDRICAL_SURFACE('',#3819,2.56);
#3373=CYLINDRICAL_SURFACE('',#3821,2.56);
#3374=CYLINDRICAL_SURFACE('',#3822,2.56);
#3375=CYLINDRICAL_SURFACE('',#3823,2.56);
#3376=CYLINDRICAL_SURFACE('',#3824,2.56);
#3377=CYLINDRICAL_SURFACE('',#3825,2.56);
#3378=CYLINDRICAL_SURFACE('',#3826,2.56);
#3379=CYLINDRICAL_SURFACE('',#3827,2.56);
#3380=CYLINDRICAL_SURFACE('',#3828,2.56);
#3381=CYLINDRICAL_SURFACE('',#3829,2.56);
#3382=CYLINDRICAL_SURFACE('',#3830,2.56);
#3383=CYLINDRICAL_SURFACE('',#3831,2.56);
#3384=CYLINDRICAL_SURFACE('',#3832,2.56);
#3385=CYLINDRICAL_SURFACE('',#3833,2.56);
#3386=CYLINDRICAL_SURFACE('',#3835,2.117);
#3387=CYLINDRICAL_SURFACE('',#3838,2.117);
#3388=CYLINDRICAL_SURFACE('',#3839,2.117);
#3389=CYLINDRICAL_SURFACE('',#3840,2.117);
#3390=CYLINDRICAL_SURFACE('',#3841,2.117);
#3391=CYLINDRICAL_SURFACE('',#3842,2.117);
#3392=CYLINDRICAL_SURFACE('',#3843,2.117);
#3393=CYLINDRICAL_SURFACE('',#3844,2.117);
#3394=CYLINDRICAL_SURFACE('',#3845,2.117);
#3395=CYLINDRICAL_SURFACE('',#3846,2.117);
#3396=CYLINDRICAL_SURFACE('',#3847,2.117);
#3397=CYLINDRICAL_SURFACE('',#3848,2.117);
#3398=CYLINDRICAL_SURFACE('',#3849,2.117);
#3399=CYLINDRICAL_SURFACE('',#3851,2.56);
#3400=CYLINDRICAL_SURFACE('',#3853,2.56);
#3401=CYLINDRICAL_SURFACE('',#3854,2.56);
#3402=CYLINDRICAL_SURFACE('',#3855,2.56);
#3403=CYLINDRICAL_SURFACE('',#3856,2.56);
#3404=CYLINDRICAL_SURFACE('',#3857,2.56);
#3405=CYLINDRICAL_SURFACE('',#3858,2.56);
#3406=CYLINDRICAL_SURFACE('',#3859,2.56);
#3407=CYLINDRICAL_SURFACE('',#3860,2.56);
#3408=CYLINDRICAL_SURFACE('',#3861,2.56);
#3409=CYLINDRICAL_SURFACE('',#3862,2.56);
#3410=CYLINDRICAL_SURFACE('',#3863,2.56);
#3411=CYLINDRICAL_SURFACE('',#3864,2.56);
#3412=CYLINDRICAL_SURFACE('',#3865,2.56);
#3413=CYLINDRICAL_SURFACE('',#3867,1.);
#3414=CYLINDRICAL_SURFACE('',#3871,1.);
#3415=CYLINDRICAL_SURFACE('',#3876,2.56);
#3416=CYLINDRICAL_SURFACE('',#3877,2.117);
#3417=CYLINDRICAL_SURFACE('',#3879,2.56);
#3418=CYLINDRICAL_SURFACE('',#3880,2.117);
#3419=CYLINDRICAL_SURFACE('',#3884,1.99999999999999);
#3420=CYLINDRICAL_SURFACE('',#3888,1.99999999999999);
#3421=CYLINDRICAL_SURFACE('',#3892,2.);
#3422=CYLINDRICAL_SURFACE('',#3896,2.);
#3423=CYLINDRICAL_SURFACE('',#3899,2.);
#3424=CYLINDRICAL_SURFACE('',#3903,2.00000000000001);
#3425=CYLINDRICAL_SURFACE('',#3911,2.00000000000001);
#3426=CYLINDRICAL_SURFACE('',#3915,2.);
#3427=CYLINDRICAL_SURFACE('',#3933,3.);
#3428=CYLINDRICAL_SURFACE('',#3936,6.);
#3429=CYLINDRICAL_SURFACE('',#3942,2.4505);
#3430=CYLINDRICAL_SURFACE('',#3944,2.4505);
#3431=CYLINDRICAL_SURFACE('',#3945,2.4505);
#3432=CYLINDRICAL_SURFACE('',#3946,2.4505);
#3433=CYLINDRICAL_SURFACE('',#3947,2.4505);
#3434=CYLINDRICAL_SURFACE('',#3948,2.4505);
#3435=CYLINDRICAL_SURFACE('',#3949,2.4505);
#3436=CYLINDRICAL_SURFACE('',#3950,2.4505);
#3437=CYLINDRICAL_SURFACE('',#3951,2.4505);
#3438=CYLINDRICAL_SURFACE('',#3952,2.4505);
#3439=CYLINDRICAL_SURFACE('',#3953,2.4505);
#3440=CYLINDRICAL_SURFACE('',#3954,2.4505);
#3441=CYLINDRICAL_SURFACE('',#3955,2.4505);
#3442=CYLINDRICAL_SURFACE('',#3956,2.4505);
#3443=CYLINDRICAL_SURFACE('',#3957,2.4505);
#3444=CYLINDRICAL_SURFACE('',#3958,2.4505);
#3445=CYLINDRICAL_SURFACE('',#3959,2.4505);
#3446=CYLINDRICAL_SURFACE('',#3960,2.4505);
#3447=CYLINDRICAL_SURFACE('',#3961,2.4505);
#3448=CYLINDRICAL_SURFACE('',#3962,2.4505);
#3449=CYLINDRICAL_SURFACE('',#3963,2.4505);
#3450=CYLINDRICAL_SURFACE('',#3964,2.4505);
#3451=CYLINDRICAL_SURFACE('',#3965,2.4505);
#3452=CYLINDRICAL_SURFACE('',#3966,2.4505);
#3453=CYLINDRICAL_SURFACE('',#3967,2.4505);
#3454=CYLINDRICAL_SURFACE('',#3968,2.4505);
#3455=CYLINDRICAL_SURFACE('',#3969,2.4505);
#3456=CYLINDRICAL_SURFACE('',#3970,2.4505);
#3457=CYLINDRICAL_SURFACE('',#3971,2.4505);
#3458=CYLINDRICAL_SURFACE('',#3972,2.4505);
#3459=CYLINDRICAL_SURFACE('',#3973,1.99475);
#3460=CYLINDRICAL_SURFACE('',#3975,1.99475);
#3461=CYLINDRICAL_SURFACE('',#3976,1.99475);
#3462=CYLINDRICAL_SURFACE('',#3977,1.99475);
#3463=CYLINDRICAL_SURFACE('',#3978,1.99475);
#3464=CYLINDRICAL_SURFACE('',#3979,1.99475);
#3465=CYLINDRICAL_SURFACE('',#3980,1.99475);
#3466=CYLINDRICAL_SURFACE('',#3981,1.99475);
#3467=CYLINDRICAL_SURFACE('',#3982,1.99475);
#3468=CYLINDRICAL_SURFACE('',#3983,1.99475);
#3469=CYLINDRICAL_SURFACE('',#3984,1.99475);
#3470=CYLINDRICAL_SURFACE('',#3985,1.99475);
#3471=CYLINDRICAL_SURFACE('',#3986,1.99475);
#3472=CYLINDRICAL_SURFACE('',#3987,1.99475);
#3473=CYLINDRICAL_SURFACE('',#3988,1.99475);
#3474=CYLINDRICAL_SURFACE('',#3989,1.99475);
#3475=CYLINDRICAL_SURFACE('',#3990,1.99475);
#3476=CYLINDRICAL_SURFACE('',#3991,1.99475);
#3477=CYLINDRICAL_SURFACE('',#3992,1.99475);
#3478=CYLINDRICAL_SURFACE('',#3993,1.99475);
#3479=CYLINDRICAL_SURFACE('',#3994,1.99475);
#3480=CYLINDRICAL_SURFACE('',#3995,1.99475);
#3481=CYLINDRICAL_SURFACE('',#3996,1.99475);
#3482=CYLINDRICAL_SURFACE('',#3997,1.99475);
#3483=CYLINDRICAL_SURFACE('',#3998,1.99475);
#3484=CYLINDRICAL_SURFACE('',#3999,1.99475);
#3485=CYLINDRICAL_SURFACE('',#4000,1.99475);
#3486=CYLINDRICAL_SURFACE('',#4001,1.99475);
#3487=CYLINDRICAL_SURFACE('',#4002,1.99475);
#3488=CYLINDRICAL_SURFACE('',#4003,1.99475);
#3489=CYLINDRICAL_SURFACE('',#4007,1.99475);
#3490=CYLINDRICAL_SURFACE('',#4009,2.4505);
#3491=CYLINDRICAL_SURFACE('',#4019,4.);
#3492=CYLINDRICAL_SURFACE('',#4024,1.);
#3493=ADVANCED_FACE('',(#417),#3351,.F.);
#3494=ADVANCED_FACE('',(#418),#365,.F.);
#3495=ADVANCED_FACE('',(#419),#3352,.F.);
#3496=ADVANCED_FACE('',(#420),#366,.F.);
#3497=ADVANCED_FACE('',(#421),#3353,.F.);
#3498=ADVANCED_FACE('',(#422),#3354,.F.);
#3499=ADVANCED_FACE('',(#423),#3355,.F.);
#3500=ADVANCED_FACE('',(#424),#3356,.F.);
#3501=ADVANCED_FACE('',(#425),#3357,.F.);
#3502=ADVANCED_FACE('',(#426),#3358,.F.);
#3503=ADVANCED_FACE('',(#427),#367,.T.);
#3504=ADVANCED_FACE('',(#428,#341,#342,#343,#344,#345,#346,#347,#348),#368,
 .T.);
#3505=ADVANCED_FACE('',(#429),#369,.T.);
#3506=ADVANCED_FACE('',(#430,#349,#350,#351,#352,#353,#354),#370,.T.);
#3507=ADVANCED_FACE('',(#431),#371,.T.);
#3508=ADVANCED_FACE('',(#432),#372,.F.);
#3509=ADVANCED_FACE('',(#433),#3359,.F.);
#3510=ADVANCED_FACE('',(#434),#3360,.F.);
#3511=ADVANCED_FACE('',(#435),#3361,.F.);
#3512=ADVANCED_FACE('',(#436),#3362,.F.);
#3513=ADVANCED_FACE('',(#437),#3363,.F.);
#3514=ADVANCED_FACE('',(#438),#3364,.F.);
#3515=ADVANCED_FACE('',(#439),#3365,.F.);
#3516=ADVANCED_FACE('',(#440),#3366,.F.);
#3517=ADVANCED_FACE('',(#441),#3367,.F.);
#3518=ADVANCED_FACE('',(#442),#3368,.F.);
#3519=ADVANCED_FACE('',(#443),#3369,.F.);
#3520=ADVANCED_FACE('',(#444),#3370,.F.);
#3521=ADVANCED_FACE('',(#445),#3371,.F.);
#3522=ADVANCED_FACE('',(#446),#3372,.F.);
#3523=ADVANCED_FACE('',(#447),#3373,.F.);
#3524=ADVANCED_FACE('',(#448),#3374,.F.);
#3525=ADVANCED_FACE('',(#449),#3375,.F.);
#3526=ADVANCED_FACE('',(#450),#3376,.F.);
#3527=ADVANCED_FACE('',(#451),#3377,.F.);
#3528=ADVANCED_FACE('',(#452),#3378,.F.);
#3529=ADVANCED_FACE('',(#453),#3379,.F.);
#3530=ADVANCED_FACE('',(#454),#3380,.F.);
#3531=ADVANCED_FACE('',(#455),#3381,.F.);
#3532=ADVANCED_FACE('',(#456),#3382,.F.);
#3533=ADVANCED_FACE('',(#457),#3383,.F.);
#3534=ADVANCED_FACE('',(#458),#3384,.F.);
#3535=ADVANCED_FACE('',(#459),#3385,.F.);
#3536=ADVANCED_FACE('',(#460),#3386,.F.);
#3537=ADVANCED_FACE('',(#461),#3387,.F.);
#3538=ADVANCED_FACE('',(#462),#3388,.F.);
#3539=ADVANCED_FACE('',(#463),#3389,.F.);
#3540=ADVANCED_FACE('',(#464),#3390,.F.);
#3541=ADVANCED_FACE('',(#465),#3391,.F.);
#3542=ADVANCED_FACE('',(#466),#3392,.F.);
#3543=ADVANCED_FACE('',(#467),#3393,.F.);
#3544=ADVANCED_FACE('',(#468),#3394,.F.);
#3545=ADVANCED_FACE('',(#469),#3395,.F.);
#3546=ADVANCED_FACE('',(#470),#3396,.F.);
#3547=ADVANCED_FACE('',(#471),#3397,.F.);
#3548=ADVANCED_FACE('',(#472),#3398,.F.);
#3549=ADVANCED_FACE('',(#473),#3399,.F.);
#3550=ADVANCED_FACE('',(#474),#3400,.F.);
#3551=ADVANCED_FACE('',(#475),#3401,.F.);
#3552=ADVANCED_FACE('',(#476),#3402,.F.);
#3553=ADVANCED_FACE('',(#477),#3403,.F.);
#3554=ADVANCED_FACE('',(#478),#3404,.F.);
#3555=ADVANCED_FACE('',(#479),#3405,.F.);
#3556=ADVANCED_FACE('',(#480),#3406,.F.);
#3557=ADVANCED_FACE('',(#481),#3407,.F.);
#3558=ADVANCED_FACE('',(#482),#3408,.F.);
#3559=ADVANCED_FACE('',(#483),#3409,.F.);
#3560=ADVANCED_FACE('',(#484),#3410,.F.);
#3561=ADVANCED_FACE('',(#485),#3411,.F.);
#3562=ADVANCED_FACE('',(#486),#3412,.F.);
#3563=ADVANCED_FACE('',(#487),#3413,.F.);
#3564=ADVANCED_FACE('',(#488),#373,.F.);
#3565=ADVANCED_FACE('',(#489),#3414,.F.);
#3566=ADVANCED_FACE('',(#490),#374,.F.);
#3567=ADVANCED_FACE('',(#491),#375,.F.);
#3568=ADVANCED_FACE('',(#492),#3415,.F.);
#3569=ADVANCED_FACE('',(#493),#56,.F.);
#3570=ADVANCED_FACE('',(#494),#57,.F.);
#3571=ADVANCED_FACE('',(#495),#3416,.F.);
#3572=ADVANCED_FACE('',(#496),#376,.F.);
#3573=ADVANCED_FACE('',(#497),#3417,.F.);
#3574=ADVANCED_FACE('',(#498),#58,.F.);
#3575=ADVANCED_FACE('',(#499),#59,.F.);
#3576=ADVANCED_FACE('',(#500),#3418,.F.);
#3577=ADVANCED_FACE('',(#501),#377,.F.);
#3578=ADVANCED_FACE('',(#502),#378,.F.);
#3579=ADVANCED_FACE('',(#503),#379,.T.);
#3580=ADVANCED_FACE('',(#504),#3419,.F.);
#3581=ADVANCED_FACE('',(#505),#380,.T.);
#3582=ADVANCED_FACE('',(#506),#3420,.F.);
#3583=ADVANCED_FACE('',(#507),#381,.T.);
#3584=ADVANCED_FACE('',(#508),#3421,.F.);
#3585=ADVANCED_FACE('',(#509),#382,.T.);
#3586=ADVANCED_FACE('',(#510),#3422,.F.);
#3587=ADVANCED_FACE('',(#511),#3423,.F.);
#3588=ADVANCED_FACE('',(#512),#383,.T.);
#3589=ADVANCED_FACE('',(#513),#3424,.F.);
#3590=ADVANCED_FACE('',(#514),#384,.T.);
#3591=ADVANCED_FACE('',(#515),#385,.T.);
#3592=ADVANCED_FACE('',(#516),#386,.T.);
#3593=ADVANCED_FACE('',(#517),#387,.T.);
#3594=ADVANCED_FACE('',(#518),#388,.T.);
#3595=ADVANCED_FACE('',(#519),#3425,.F.);
#3596=ADVANCED_FACE('',(#520),#389,.T.);
#3597=ADVANCED_FACE('',(#521),#3426,.F.);
#3598=ADVANCED_FACE('',(#522),#390,.T.);
#3599=ADVANCED_FACE('',(#523),#391,.T.);
#3600=ADVANCED_FACE('',(#524,#355,#356,#357,#358),#392,.T.);
#3601=ADVANCED_FACE('',(#525),#393,.T.);
#3602=ADVANCED_FACE('',(#526),#394,.T.);
#3603=ADVANCED_FACE('',(#527,#359),#395,.T.);
#3604=ADVANCED_FACE('',(#528,#360),#396,.F.);
#3605=ADVANCED_FACE('',(#529),#397,.T.);
#3606=ADVANCED_FACE('',(#530),#398,.T.);
#3607=ADVANCED_FACE('',(#531),#399,.T.);
#3608=ADVANCED_FACE('',(#532),#400,.T.);
#3609=ADVANCED_FACE('',(#533),#401,.T.);
#3610=ADVANCED_FACE('',(#534),#402,.F.);
#3611=ADVANCED_FACE('',(#535),#3427,.F.);
#3612=ADVANCED_FACE('',(#536),#3428,.T.);
#3613=ADVANCED_FACE('',(#537,#361),#403,.T.);
#3614=ADVANCED_FACE('',(#538,#362),#404,.F.);
#3615=ADVANCED_FACE('',(#539),#3429,.T.);
#3616=ADVANCED_FACE('',(#540),#3430,.T.);
#3617=ADVANCED_FACE('',(#541),#3431,.T.);
#3618=ADVANCED_FACE('',(#542),#3432,.T.);
#3619=ADVANCED_FACE('',(#543),#3433,.T.);
#3620=ADVANCED_FACE('',(#544),#3434,.T.);
#3621=ADVANCED_FACE('',(#545),#3435,.T.);
#3622=ADVANCED_FACE('',(#546),#3436,.T.);
#3623=ADVANCED_FACE('',(#547),#3437,.T.);
#3624=ADVANCED_FACE('',(#548),#3438,.T.);
#3625=ADVANCED_FACE('',(#549),#3439,.T.);
#3626=ADVANCED_FACE('',(#550),#3440,.T.);
#3627=ADVANCED_FACE('',(#551),#3441,.T.);
#3628=ADVANCED_FACE('',(#552),#3442,.T.);
#3629=ADVANCED_FACE('',(#553),#3443,.T.);
#3630=ADVANCED_FACE('',(#554),#3444,.T.);
#3631=ADVANCED_FACE('',(#555),#3445,.T.);
#3632=ADVANCED_FACE('',(#556),#3446,.T.);
#3633=ADVANCED_FACE('',(#557),#3447,.T.);
#3634=ADVANCED_FACE('',(#558),#3448,.T.);
#3635=ADVANCED_FACE('',(#559),#3449,.T.);
#3636=ADVANCED_FACE('',(#560),#3450,.T.);
#3637=ADVANCED_FACE('',(#561),#3451,.T.);
#3638=ADVANCED_FACE('',(#562),#3452,.T.);
#3639=ADVANCED_FACE('',(#563),#3453,.T.);
#3640=ADVANCED_FACE('',(#564),#3454,.T.);
#3641=ADVANCED_FACE('',(#565),#3455,.T.);
#3642=ADVANCED_FACE('',(#566),#3456,.T.);
#3643=ADVANCED_FACE('',(#567),#3457,.T.);
#3644=ADVANCED_FACE('',(#568),#3458,.T.);
#3645=ADVANCED_FACE('',(#569),#3459,.T.);
#3646=ADVANCED_FACE('',(#570),#3460,.T.);
#3647=ADVANCED_FACE('',(#571),#3461,.T.);
#3648=ADVANCED_FACE('',(#572),#3462,.T.);
#3649=ADVANCED_FACE('',(#573),#3463,.T.);
#3650=ADVANCED_FACE('',(#574),#3464,.T.);
#3651=ADVANCED_FACE('',(#575),#3465,.T.);
#3652=ADVANCED_FACE('',(#576),#3466,.T.);
#3653=ADVANCED_FACE('',(#577),#3467,.T.);
#3654=ADVANCED_FACE('',(#578),#3468,.T.);
#3655=ADVANCED_FACE('',(#579),#3469,.T.);
#3656=ADVANCED_FACE('',(#580),#3470,.T.);
#3657=ADVANCED_FACE('',(#581),#3471,.T.);
#3658=ADVANCED_FACE('',(#582),#3472,.T.);
#3659=ADVANCED_FACE('',(#583),#3473,.T.);
#3660=ADVANCED_FACE('',(#584),#3474,.T.);
#3661=ADVANCED_FACE('',(#585),#3475,.T.);
#3662=ADVANCED_FACE('',(#586),#3476,.T.);
#3663=ADVANCED_FACE('',(#587),#3477,.T.);
#3664=ADVANCED_FACE('',(#588),#3478,.T.);
#3665=ADVANCED_FACE('',(#589),#3479,.T.);
#3666=ADVANCED_FACE('',(#590),#3480,.T.);
#3667=ADVANCED_FACE('',(#591),#3481,.T.);
#3668=ADVANCED_FACE('',(#592),#3482,.T.);
#3669=ADVANCED_FACE('',(#593),#3483,.T.);
#3670=ADVANCED_FACE('',(#594),#3484,.T.);
#3671=ADVANCED_FACE('',(#595),#3485,.T.);
#3672=ADVANCED_FACE('',(#596),#3486,.T.);
#3673=ADVANCED_FACE('',(#597),#3487,.T.);
#3674=ADVANCED_FACE('',(#598),#3488,.T.);
#3675=ADVANCED_FACE('',(#599),#55,.T.);
#3676=ADVANCED_FACE('',(#600),#60,.F.);
#3677=ADVANCED_FACE('',(#601),#3489,.T.);
#3678=ADVANCED_FACE('',(#602),#61,.F.);
#3679=ADVANCED_FACE('',(#603),#3490,.T.);
#3680=ADVANCED_FACE('',(#604),#405,.F.);
#3681=ADVANCED_FACE('',(#605),#406,.F.);
#3682=ADVANCED_FACE('',(#606),#407,.F.);
#3683=ADVANCED_FACE('',(#607),#408,.F.);
#3684=ADVANCED_FACE('',(#608),#409,.F.);
#3685=ADVANCED_FACE('',(#609),#410,.F.);
#3686=ADVANCED_FACE('',(#610),#411,.F.);
#3687=ADVANCED_FACE('',(#611,#363),#412,.T.);
#3688=ADVANCED_FACE('',(#612),#3491,.T.);
#3689=ADVANCED_FACE('',(#613,#364),#413,.F.);
#3690=ADVANCED_FACE('',(#614),#414,.T.);
#3691=ADVANCED_FACE('',(#615),#3492,.T.);
#3692=ADVANCED_FACE('',(#616),#415,.T.);
#3693=ADVANCED_FACE('',(#617),#416,.F.);
#3694=CLOSED_SHELL('',(#3493,#3494,#3495,#3496,#3497,#3498,#3499,#3500,
#3501,#3502,#3503,#3504,#3505,#3506,#3507,#3508));
#3695=CLOSED_SHELL('',(#3509,#3510,#3511,#3512,#3513,#3514,#3515,#3516,
#3517,#3518,#3519,#3520,#3521,#3522,#3523,#3524,#3525,#3526,#3527,#3528,
#3529,#3530,#3531,#3532,#3533,#3534,#3535,#3536,#3537,#3538,#3539,#3540,
#3541,#3542,#3543,#3544,#3545,#3546,#3547,#3548,#3549,#3550,#3551,#3552,
#3553,#3554,#3555,#3556,#3557,#3558,#3559,#3560,#3561,#3562,#3563,#3564,
#3565,#3566,#3567,#3568,#3569,#3570,#3571,#3572,#3573,#3574,#3575,#3576,
#3577,#3578,#3579,#3580,#3581,#3582,#3583,#3584,#3585,#3586,#3587,#3588,
#3589,#3590,#3591,#3592,#3593,#3594,#3595,#3596,#3597,#3598,#3599,#3600,
#3601,#3602,#3603,#3604));
#3696=CLOSED_SHELL('',(#3605,#3606,#3607,#3608,#3609,#3610));
#3697=CLOSED_SHELL('',(#3611,#3612,#3613,#3614));
#3698=CLOSED_SHELL('',(#3615,#3616,#3617,#3618,#3619,#3620,#3621,#3622,
#3623,#3624,#3625,#3626,#3627,#3628,#3629,#3630,#3631,#3632,#3633,#3634,
#3635,#3636,#3637,#3638,#3639,#3640,#3641,#3642,#3643,#3644,#3645,#3646,
#3647,#3648,#3649,#3650,#3651,#3652,#3653,#3654,#3655,#3656,#3657,#3658,
#3659,#3660,#3661,#3662,#3663,#3664,#3665,#3666,#3667,#3668,#3669,#3670,
#3671,#3672,#3673,#3674,#3675,#3676,#3677,#3678,#3679,#3680,#3681,#3682,
#3683,#3684,#3685,#3686,#3687,#3688,#3689,#3690));
#3699=CLOSED_SHELL('',(#3691,#3692,#3693));
#3700=DERIVED_UNIT_ELEMENT(#3712,1.);
#3701=DERIVED_UNIT_ELEMENT(#13803,-3.);
#3702=DERIVED_UNIT_ELEMENT(#3712,1.);
#3703=DERIVED_UNIT_ELEMENT(#13803,-3.);
#3704=DERIVED_UNIT_ELEMENT(#3712,1.);
#3705=DERIVED_UNIT_ELEMENT(#13803,-3.);
#3706=DERIVED_UNIT_ELEMENT(#3712,1.);
#3707=DERIVED_UNIT_ELEMENT(#13803,-3.);
#3708=DERIVED_UNIT_ELEMENT(#3712,1.);
#3709=DERIVED_UNIT_ELEMENT(#13803,-3.);
#3710=DERIVED_UNIT_ELEMENT(#3712,1.);
#3711=DERIVED_UNIT_ELEMENT(#13803,-3.);
#3712=(
MASS_UNIT()
NAMED_UNIT(*)
SI_UNIT(.KILO.,.GRAM.)
);
#3713=DERIVED_UNIT((#3700,#3701));
#3714=DERIVED_UNIT((#3702,#3703));
#3715=DERIVED_UNIT((#3704,#3705));
#3716=DERIVED_UNIT((#3706,#3707));
#3717=DERIVED_UNIT((#3708,#3709));
#3718=DERIVED_UNIT((#3710,#3711));
#3719=MEASURE_REPRESENTATION_ITEM('density measure',
POSITIVE_RATIO_MEASURE(7850.),#3713);
#3720=MEASURE_REPRESENTATION_ITEM('density measure',
POSITIVE_RATIO_MEASURE(7850.),#3714);
#3721=MEASURE_REPRESENTATION_ITEM('density measure',
POSITIVE_RATIO_MEASURE(1250.),#3715);
#3722=MEASURE_REPRESENTATION_ITEM('density measure',
POSITIVE_RATIO_MEASURE(7850.),#3716);
#3723=MEASURE_REPRESENTATION_ITEM('density measure',
POSITIVE_RATIO_MEASURE(7850.),#3717);
#3724=MEASURE_REPRESENTATION_ITEM('density measure',
POSITIVE_RATIO_MEASURE(7850.),#3718);
#3725=PROPERTY_DEFINITION_REPRESENTATION(#3755,#3737);
#3726=PROPERTY_DEFINITION_REPRESENTATION(#3756,#3738);
#3727=PROPERTY_DEFINITION_REPRESENTATION(#3757,#3739);
#3728=PROPERTY_DEFINITION_REPRESENTATION(#3758,#3740);
#3729=PROPERTY_DEFINITION_REPRESENTATION(#3759,#3741);
#3730=PROPERTY_DEFINITION_REPRESENTATION(#3760,#3742);
#3731=PROPERTY_DEFINITION_REPRESENTATION(#3761,#3743);
#3732=PROPERTY_DEFINITION_REPRESENTATION(#3762,#3744);
#3733=PROPERTY_DEFINITION_REPRESENTATION(#3763,#3745);
#3734=PROPERTY_DEFINITION_REPRESENTATION(#3764,#3746);
#3735=PROPERTY_DEFINITION_REPRESENTATION(#3765,#3747);
#3736=PROPERTY_DEFINITION_REPRESENTATION(#3766,#3748);
#3737=REPRESENTATION('material name',(#3749),#13795);
#3738=REPRESENTATION('density',(#3719),#13795);
#3739=REPRESENTATION('material name',(#3750),#13796);
#3740=REPRESENTATION('density',(#3720),#13796);
#3741=REPRESENTATION('material name',(#3751),#13797);
#3742=REPRESENTATION('density',(#3721),#13797);
#3743=REPRESENTATION('material name',(#3752),#13798);
#3744=REPRESENTATION('density',(#3722),#13798);
#3745=REPRESENTATION('material name',(#3753),#13799);
#3746=REPRESENTATION('density',(#3723),#13799);
#3747=REPRESENTATION('material name',(#3754),#13800);
#3748=REPRESENTATION('density',(#3724),#13800);
#3749=DESCRIPTIVE_REPRESENTATION_ITEM('Steel','Steel');
#3750=DESCRIPTIVE_REPRESENTATION_ITEM('Steel','Steel');
#3751=DESCRIPTIVE_REPRESENTATION_ITEM('Rubber, Silicone',
'Rubber, Silicone');
#3752=DESCRIPTIVE_REPRESENTATION_ITEM('Steel','Steel');
#3753=DESCRIPTIVE_REPRESENTATION_ITEM('Steel','Steel');
#3754=DESCRIPTIVE_REPRESENTATION_ITEM('Steel','Steel');
#3755=PROPERTY_DEFINITION('material property','material name',#13844);
#3756=PROPERTY_DEFINITION('material property','density of part',#13844);
#3757=PROPERTY_DEFINITION('material property','material name',#13845);
#3758=PROPERTY_DEFINITION('material property','density of part',#13845);
#3759=PROPERTY_DEFINITION('material property','material name',#13846);
#3760=PROPERTY_DEFINITION('material property','density of part',#13846);
#3761=PROPERTY_DEFINITION('material property','material name',#13847);
#3762=PROPERTY_DEFINITION('material property','density of part',#13847);
#3763=PROPERTY_DEFINITION('material property','material name',#13848);
#3764=PROPERTY_DEFINITION('material property','density of part',#13848);
#3765=PROPERTY_DEFINITION('material property','material name',#13849);
#3766=PROPERTY_DEFINITION('material property','density of part',#13849);
#3767=AXIS2_PLACEMENT_3D('',#4815,#4040,#4041);
#3768=AXIS2_PLACEMENT_3D('',#4816,#4042,#4043);
#3769=AXIS2_PLACEMENT_3D('',#4817,#4044,#4045);
#3770=AXIS2_PLACEMENT_3D('',#4818,#4046,#4047);
#3771=AXIS2_PLACEMENT_3D('',#4820,#4048,#4049);
#3772=AXIS2_PLACEMENT_3D('',#4823,#4051,#4052);
#3773=AXIS2_PLACEMENT_3D('',#4824,#4053,#4054);
#3774=AXIS2_PLACEMENT_3D('',#4825,#4055,#4056);
#3775=AXIS2_PLACEMENT_3D('',#4827,#4057,#4058);
#3776=AXIS2_PLACEMENT_3D('',#4830,#4060,#4061);
#3777=AXIS2_PLACEMENT_3D('',#4831,#4062,#4063);
#3778=AXIS2_PLACEMENT_3D('',#4832,#4064,#4065);
#3779=AXIS2_PLACEMENT_3D('',#4834,#4066,#4067);
#3780=AXIS2_PLACEMENT_3D('',#4837,#4069,#4070);
#3781=AXIS2_PLACEMENT_3D('',#4838,#4071,#4072);
#3782=AXIS2_PLACEMENT_3D('',#4840,#4073,#4074);
#3783=AXIS2_PLACEMENT_3D('',#4843,#4076,#4077);
#3784=AXIS2_PLACEMENT_3D('',#4844,#4078,#4079);
#3785=AXIS2_PLACEMENT_3D('',#4846,#4080,#4081);
#3786=AXIS2_PLACEMENT_3D('',#4849,#4083,#4084);
#3787=AXIS2_PLACEMENT_3D('',#4850,#4085,#4086);
#3788=AXIS2_PLACEMENT_3D('',#4852,#4087,#4088);
#3789=AXIS2_PLACEMENT_3D('',#4855,#4090,#4091);
#3790=AXIS2_PLACEMENT_3D('',#4856,#4092,#4093);
#3791=AXIS2_PLACEMENT_3D('',#4858,#4094,#4095);
#3792=AXIS2_PLACEMENT_3D('',#4861,#4097,#4098);
#3793=AXIS2_PLACEMENT_3D('',#4862,#4099,#4100);
#3794=AXIS2_PLACEMENT_3D('',#4864,#4101,#4102);
#3795=AXIS2_PLACEMENT_3D('',#4867,#4104,#4105);
#3796=AXIS2_PLACEMENT_3D('',#4868,#4106,#4107);
#3797=AXIS2_PLACEMENT_3D('',#4877,#4112,#4113);
#3798=AXIS2_PLACEMENT_3D('',#4883,#4117,#4118);
#3799=AXIS2_PLACEMENT_3D('',#4889,#4122,#4123);
#3800=AXIS2_PLACEMENT_3D('',#4892,#4126,#4127);
#3801=AXIS2_PLACEMENT_3D('',#4893,#4128,#4129);
#3802=AXIS2_PLACEMENT_3D('',#4894,#4130,#4131);
#3803=AXIS2_PLACEMENT_3D('',#4895,#4132,#4133);
#3804=AXIS2_PLACEMENT_3D('',#4920,#4135,#4136);
#3805=AXIS2_PLACEMENT_3D('',#4928,#4138,#4139);
#3806=AXIS2_PLACEMENT_3D('',#4954,#4140,#4141);
#3807=AXIS2_PLACEMENT_3D('',#5002,#4143,#4144);
#3808=AXIS2_PLACEMENT_3D('',#5053,#4146,#4147);
#3809=AXIS2_PLACEMENT_3D('',#5104,#4149,#4150);
#3810=AXIS2_PLACEMENT_3D('',#5152,#4152,#4153);
#3811=AXIS2_PLACEMENT_3D('',#5203,#4155,#4156);
#3812=AXIS2_PLACEMENT_3D('',#5254,#4158,#4159);
#3813=AXIS2_PLACEMENT_3D('',#5302,#4161,#4162);
#3814=AXIS2_PLACEMENT_3D('',#5353,#4164,#4165);
#3815=AXIS2_PLACEMENT_3D('',#5404,#4167,#4168);
#3816=AXIS2_PLACEMENT_3D('',#5452,#4170,#4171);
#3817=AXIS2_PLACEMENT_3D('',#5503,#4173,#4174);
#3818=AXIS2_PLACEMENT_3D('',#5522,#4176,#4177);
#3819=AXIS2_PLACEMENT_3D('',#5542,#4178,#4179);
#3820=AXIS2_PLACEMENT_3D('',#5554,#4181,#4182);
#3821=AXIS2_PLACEMENT_3D('',#5562,#4183,#4184);
#3822=AXIS2_PLACEMENT_3D('',#5587,#4186,#4187);
#3823=AXIS2_PLACEMENT_3D('',#5612,#4189,#4190);
#3824=AXIS2_PLACEMENT_3D('',#5636,#4192,#4193);
#3825=AXIS2_PLACEMENT_3D('',#5661,#4195,#4196);
#3826=AXIS2_PLACEMENT_3D('',#5686,#4198,#4199);
#3827=AXIS2_PLACEMENT_3D('',#5710,#4201,#4202);
#3828=AXIS2_PLACEMENT_3D('',#5735,#4204,#4205);
#3829=AXIS2_PLACEMENT_3D('',#5760,#4207,#4208);
#3830=AXIS2_PLACEMENT_3D('',#5784,#4210,#4211);
#3831=AXIS2_PLACEMENT_3D('',#5809,#4213,#4214);
#3832=AXIS2_PLACEMENT_3D('',#5834,#4216,#4217);
#3833=AXIS2_PLACEMENT_3D('',#5858,#4219,#4220);
#3834=AXIS2_PLACEMENT_3D('',#5869,#4222,#4223);
#3835=AXIS2_PLACEMENT_3D('',#5875,#4224,#4225);
#3836=AXIS2_PLACEMENT_3D('',#5900,#4227,#4228);
#3837=AXIS2_PLACEMENT_3D('',#5908,#4230,#4231);
#3838=AXIS2_PLACEMENT_3D('',#5934,#4232,#4233);
#3839=AXIS2_PLACEMENT_3D('',#5982,#4235,#4236);
#3840=AXIS2_PLACEMENT_3D('',#6033,#4238,#4239);
#3841=AXIS2_PLACEMENT_3D('',#6084,#4241,#4242);
#3842=AXIS2_PLACEMENT_3D('',#6132,#4244,#4245);
#3843=AXIS2_PLACEMENT_3D('',#6183,#4247,#4248);
#3844=AXIS2_PLACEMENT_3D('',#6234,#4250,#4251);
#3845=AXIS2_PLACEMENT_3D('',#6282,#4253,#4254);
#3846=AXIS2_PLACEMENT_3D('',#6333,#4256,#4257);
#3847=AXIS2_PLACEMENT_3D('',#6384,#4259,#4260);
#3848=AXIS2_PLACEMENT_3D('',#6432,#4262,#4263);
#3849=AXIS2_PLACEMENT_3D('',#6483,#4265,#4266);
#3850=AXIS2_PLACEMENT_3D('',#6502,#4268,#4269);
#3851=AXIS2_PLACEMENT_3D('',#6522,#4270,#4271);
#3852=AXIS2_PLACEMENT_3D('',#6534,#4273,#4274);
#3853=AXIS2_PLACEMENT_3D('',#6542,#4275,#4276);
#3854=AXIS2_PLACEMENT_3D('',#6567,#4278,#4279);
#3855=AXIS2_PLACEMENT_3D('',#6592,#4281,#4282);
#3856=AXIS2_PLACEMENT_3D('',#6616,#4284,#4285);
#3857=AXIS2_PLACEMENT_3D('',#6641,#4287,#4288);
#3858=AXIS2_PLACEMENT_3D('',#6666,#4290,#4291);
#3859=AXIS2_PLACEMENT_3D('',#6690,#4293,#4294);
#3860=AXIS2_PLACEMENT_3D('',#6715,#4296,#4297);
#3861=AXIS2_PLACEMENT_3D('',#6740,#4299,#4300);
#3862=AXIS2_PLACEMENT_3D('',#6764,#4302,#4303);
#3863=AXIS2_PLACEMENT_3D('',#6789,#4305,#4306);
#3864=AXIS2_PLACEMENT_3D('',#6814,#4308,#4309);
#3865=AXIS2_PLACEMENT_3D('',#6838,#4311,#4312);
#3866=AXIS2_PLACEMENT_3D('',#6849,#4314,#4315);
#3867=AXIS2_PLACEMENT_3D('',#6855,#4316,#4317);
#3868=AXIS2_PLACEMENT_3D('',#6857,#4318,#4319);
#3869=AXIS2_PLACEMENT_3D('',#6860,#4321,#4322);
#3870=AXIS2_PLACEMENT_3D('',#6861,#4323,#4324);
#3871=AXIS2_PLACEMENT_3D('',#6862,#4325,#4326);
#3872=AXIS2_PLACEMENT_3D('',#6864,#4327,#4328);
#3873=AXIS2_PLACEMENT_3D('',#6867,#4330,#4331);
#3874=AXIS2_PLACEMENT_3D('',#6868,#4332,#4333);
#3875=AXIS2_PLACEMENT_3D('',#6869,#4334,#4335);
#3876=AXIS2_PLACEMENT_3D('',#7049,#4336,#4337);
#3877=AXIS2_PLACEMENT_3D('',#8036,#4338,#4339);
#3878=AXIS2_PLACEMENT_3D('',#8037,#4340,#4341);
#3879=AXIS2_PLACEMENT_3D('',#8217,#4342,#4343);
#3880=AXIS2_PLACEMENT_3D('',#9204,#4344,#4345);
#3881=AXIS2_PLACEMENT_3D('',#9205,#4346,#4347);
#3882=AXIS2_PLACEMENT_3D('',#9206,#4348,#4349);
#3883=AXIS2_PLACEMENT_3D('',#9207,#4350,#4351);
#3884=AXIS2_PLACEMENT_3D('',#9216,#4356,#4357);
#3885=AXIS2_PLACEMENT_3D('',#9218,#4358,#4359);
#3886=AXIS2_PLACEMENT_3D('',#9220,#4360,#4361);
#3887=AXIS2_PLACEMENT_3D('',#9222,#4363,#4364);
#3888=AXIS2_PLACEMENT_3D('',#9228,#4368,#4369);
#3889=AXIS2_PLACEMENT_3D('',#9230,#4370,#4371);
#3890=AXIS2_PLACEMENT_3D('',#9232,#4372,#4373);
#3891=AXIS2_PLACEMENT_3D('',#9234,#4375,#4376);
#3892=AXIS2_PLACEMENT_3D('',#9240,#4380,#4381);
#3893=AXIS2_PLACEMENT_3D('',#9242,#4382,#4383);
#3894=AXIS2_PLACEMENT_3D('',#9244,#4384,#4385);
#3895=AXIS2_PLACEMENT_3D('',#9246,#4387,#4388);
#3896=AXIS2_PLACEMENT_3D('',#9252,#4392,#4393);
#3897=AXIS2_PLACEMENT_3D('',#9253,#4394,#4395);
#3898=AXIS2_PLACEMENT_3D('',#9254,#4396,#4397);
#3899=AXIS2_PLACEMENT_3D('',#9255,#4398,#4399);
#3900=AXIS2_PLACEMENT_3D('',#9258,#4400,#4401);
#3901=AXIS2_PLACEMENT_3D('',#9262,#4403,#4404);
#3902=AXIS2_PLACEMENT_3D('',#9264,#4406,#4407);
#3903=AXIS2_PLACEMENT_3D('',#9270,#4411,#4412);
#3904=AXIS2_PLACEMENT_3D('',#9272,#4413,#4414);
#3905=AXIS2_PLACEMENT_3D('',#9274,#4415,#4416);
#3906=AXIS2_PLACEMENT_3D('',#9276,#4418,#4419);
#3907=AXIS2_PLACEMENT_3D('',#9282,#4423,#4424);
#3908=AXIS2_PLACEMENT_3D('',#9288,#4428,#4429);
#3909=AXIS2_PLACEMENT_3D('',#9294,#4433,#4434);
#3910=AXIS2_PLACEMENT_3D('',#9300,#4438,#4439);
#3911=AXIS2_PLACEMENT_3D('',#9306,#4443,#4444);
#3912=AXIS2_PLACEMENT_3D('',#9308,#4445,#4446);
#3913=AXIS2_PLACEMENT_3D('',#9310,#4447,#4448);
#3914=AXIS2_PLACEMENT_3D('',#9312,#4450,#4451);
#3915=AXIS2_PLACEMENT_3D('',#9318,#4455,#4456);
#3916=AXIS2_PLACEMENT_3D('',#9320,#4457,#4458);
#3917=AXIS2_PLACEMENT_3D('',#9322,#4459,#4460);
#3918=AXIS2_PLACEMENT_3D('',#9324,#4462,#4463);
#3919=AXIS2_PLACEMENT_3D('',#9330,#4467,#4468);
#3920=AXIS2_PLACEMENT_3D('',#9336,#4472,#4473);
#3921=AXIS2_PLACEMENT_3D('',#9342,#4477,#4478);
#3922=AXIS2_PLACEMENT_3D('',#9348,#4482,#4483);
#3923=AXIS2_PLACEMENT_3D('',#9351,#4486,#4487);
#3924=AXIS2_PLACEMENT_3D('',#9352,#4488,#4489);
#3925=AXIS2_PLACEMENT_3D('',#9353,#4490,#4491);
#3926=AXIS2_PLACEMENT_3D('',#9354,#4492,#4493);
#3927=AXIS2_PLACEMENT_3D('',#9363,#4498,#4499);
#3928=AXIS2_PLACEMENT_3D('',#9369,#4503,#4504);
#3929=AXIS2_PLACEMENT_3D('',#9375,#4508,#4509);
#3930=AXIS2_PLACEMENT_3D('',#9378,#4512,#4513);
#3931=AXIS2_PLACEMENT_3D('',#9379,#4514,#4515);
#3932=AXIS2_PLACEMENT_3D('',#9380,#4516,#4517);
#3933=AXIS2_PLACEMENT_3D('',#9381,#4518,#4519);
#3934=AXIS2_PLACEMENT_3D('',#9383,#4520,#4521);
#3935=AXIS2_PLACEMENT_3D('',#9386,#4523,#4524);
#3936=AXIS2_PLACEMENT_3D('',#9387,#4525,#4526);
#3937=AXIS2_PLACEMENT_3D('',#9389,#4527,#4528);
#3938=AXIS2_PLACEMENT_3D('',#9392,#4530,#4531);
#3939=AXIS2_PLACEMENT_3D('',#9393,#4532,#4533);
#3940=AXIS2_PLACEMENT_3D('',#9394,#4534,#4535);
#3941=AXIS2_PLACEMENT_3D('',#9395,#4536,#4537);
#3942=AXIS2_PLACEMENT_3D('',#9396,#4538,#4539);
#3943=AXIS2_PLACEMENT_3D('',#9412,#4541,#4542);
#3944=AXIS2_PLACEMENT_3D('',#9420,#4543,#4544);
#3945=AXIS2_PLACEMENT_3D('',#9468,#4546,#4547);
#3946=AXIS2_PLACEMENT_3D('',#9516,#4549,#4550);
#3947=AXIS2_PLACEMENT_3D('',#9570,#4552,#4553);
#3948=AXIS2_PLACEMENT_3D('',#9618,#4555,#4556);
#3949=AXIS2_PLACEMENT_3D('',#9666,#4558,#4559);
#3950=AXIS2_PLACEMENT_3D('',#9714,#4561,#4562);
#3951=AXIS2_PLACEMENT_3D('',#9768,#4564,#4565);
#3952=AXIS2_PLACEMENT_3D('',#9816,#4567,#4568);
#3953=AXIS2_PLACEMENT_3D('',#9864,#4570,#4571);
#3954=AXIS2_PLACEMENT_3D('',#9918,#4573,#4574);
#3955=AXIS2_PLACEMENT_3D('',#9966,#4576,#4577);
#3956=AXIS2_PLACEMENT_3D('',#10014,#4579,#4580);
#3957=AXIS2_PLACEMENT_3D('',#10065,#4582,#4583);
#3958=AXIS2_PLACEMENT_3D('',#10113,#4585,#4586);
#3959=AXIS2_PLACEMENT_3D('',#10161,#4588,#4589);
#3960=AXIS2_PLACEMENT_3D('',#10209,#4591,#4592);
#3961=AXIS2_PLACEMENT_3D('',#10263,#4594,#4595);
#3962=AXIS2_PLACEMENT_3D('',#10311,#4597,#4598);
#3963=AXIS2_PLACEMENT_3D('',#10359,#4600,#4601);
#3964=AXIS2_PLACEMENT_3D('',#10413,#4603,#4604);
#3965=AXIS2_PLACEMENT_3D('',#10461,#4606,#4607);
#3966=AXIS2_PLACEMENT_3D('',#10509,#4609,#4610);
#3967=AXIS2_PLACEMENT_3D('',#10560,#4612,#4613);
#3968=AXIS2_PLACEMENT_3D('',#10611,#4615,#4616);
#3969=AXIS2_PLACEMENT_3D('',#10659,#4618,#4619);
#3970=AXIS2_PLACEMENT_3D('',#10707,#4621,#4622);
#3971=AXIS2_PLACEMENT_3D('',#10761,#4624,#4625);
#3972=AXIS2_PLACEMENT_3D('',#10809,#4627,#4628);
#3973=AXIS2_PLACEMENT_3D('',#10857,#4630,#4631);
#3974=AXIS2_PLACEMENT_3D('',#10873,#4633,#4634);
#3975=AXIS2_PLACEMENT_3D('',#10882,#4635,#4636);
#3976=AXIS2_PLACEMENT_3D('',#10907,#4638,#4639);
#3977=AXIS2_PLACEMENT_3D('',#10931,#4641,#4642);
#3978=AXIS2_PLACEMENT_3D('',#10956,#4644,#4645);
#3979=AXIS2_PLACEMENT_3D('',#10981,#4647,#4648);
#3980=AXIS2_PLACEMENT_3D('',#11005,#4650,#4651);
#3981=AXIS2_PLACEMENT_3D('',#11029,#4653,#4654);
#3982=AXIS2_PLACEMENT_3D('',#11055,#4656,#4657);
#3983=AXIS2_PLACEMENT_3D('',#11079,#4659,#4660);
#3984=AXIS2_PLACEMENT_3D('',#11103,#4662,#4663);
#3985=AXIS2_PLACEMENT_3D('',#11128,#4665,#4666);
#3986=AXIS2_PLACEMENT_3D('',#11153,#4668,#4669);
#3987=AXIS2_PLACEMENT_3D('',#11177,#4671,#4672);
#3988=AXIS2_PLACEMENT_3D('',#11202,#4674,#4675);
#3989=AXIS2_PLACEMENT_3D('',#11227,#4677,#4678);
#3990=AXIS2_PLACEMENT_3D('',#11251,#4680,#4681);
#3991=AXIS2_PLACEMENT_3D('',#11275,#4683,#4684);
#3992=AXIS2_PLACEMENT_3D('',#11301,#4686,#4687);
#3993=AXIS2_PLACEMENT_3D('',#11325,#4689,#4690);
#3994=AXIS2_PLACEMENT_3D('',#11349,#4692,#4693);
#3995=AXIS2_PLACEMENT_3D('',#11374,#4695,#4696);
#3996=AXIS2_PLACEMENT_3D('',#11399,#4698,#4699);
#3997=AXIS2_PLACEMENT_3D('',#11423,#4701,#4702);
#3998=AXIS2_PLACEMENT_3D('',#11448,#4704,#4705);
#3999=AXIS2_PLACEMENT_3D('',#11473,#4707,#4708);
#4000=AXIS2_PLACEMENT_3D('',#11497,#4710,#4711);
#4001=AXIS2_PLACEMENT_3D('',#11521,#4713,#4714);
#4002=AXIS2_PLACEMENT_3D('',#11546,#4716,#4717);
#4003=AXIS2_PLACEMENT_3D('',#11571,#4719,#4720);
#4004=AXIS2_PLACEMENT_3D('',#11595,#4722,#4723);
#4005=AXIS2_PLACEMENT_3D('',#11874,#4724,#4725);
#4006=AXIS2_PLACEMENT_3D('',#11905,#4727,#4728);
#4007=AXIS2_PLACEMENT_3D('',#12806,#4729,#4730);
#4008=AXIS2_PLACEMENT_3D('',#12817,#4731,#4732);
#4009=AXIS2_PLACEMENT_3D('',#13717,#4733,#4734);
#4010=AXIS2_PLACEMENT_3D('',#13718,#4735,#4736);
#4011=AXIS2_PLACEMENT_3D('',#13727,#4741,#4742);
#4012=AXIS2_PLACEMENT_3D('',#13733,#4746,#4747);
#4013=AXIS2_PLACEMENT_3D('',#13739,#4751,#4752);
#4014=AXIS2_PLACEMENT_3D('',#13745,#4756,#4757);
#4015=AXIS2_PLACEMENT_3D('',#13751,#4761,#4762);
#4016=AXIS2_PLACEMENT_3D('',#13754,#4765,#4766);
#4017=AXIS2_PLACEMENT_3D('',#13755,#4767,#4768);
#4018=AXIS2_PLACEMENT_3D('',#13757,#4769,#4770);
#4019=AXIS2_PLACEMENT_3D('',#13758,#4771,#4772);
#4020=AXIS2_PLACEMENT_3D('',#13761,#4774,#4775);
#4021=AXIS2_PLACEMENT_3D('',#13762,#4776,#4777);
#4022=AXIS2_PLACEMENT_3D('',#13763,#4778,#4779);
#4023=AXIS2_PLACEMENT_3D('',#13764,#4780,#4781);
#4024=AXIS2_PLACEMENT_3D('',#13765,#4782,#4783);
#4025=AXIS2_PLACEMENT_3D('',#13767,#4784,#4785);
#4026=AXIS2_PLACEMENT_3D('',#13770,#4787,#4788);
#4027=AXIS2_PLACEMENT_3D('',#13771,#4789,#4790);
#4028=AXIS2_PLACEMENT_3D('',#13772,#4791,#4792);
#4029=AXIS2_PLACEMENT_3D('',#13773,#4793,#4794);
#4030=AXIS2_PLACEMENT_3D('',#13774,#4795,#4796);
#4031=AXIS2_PLACEMENT_3D('',#13775,#4797,#4798);
#4032=AXIS2_PLACEMENT_3D('',#13776,#4799,#4800);
#4033=AXIS2_PLACEMENT_3D('',#13777,#4801,#4802);
#4034=AXIS2_PLACEMENT_3D('',#13778,#4803,#4804);
#4035=AXIS2_PLACEMENT_3D('',#13779,#4805,#4806);
#4036=AXIS2_PLACEMENT_3D('',#13780,#4807,#4808);
#4037=AXIS2_PLACEMENT_3D('',#13781,#4809,#4810);
#4038=AXIS2_PLACEMENT_3D('',#13782,#4811,#4812);
#4039=AXIS2_PLACEMENT_3D('',#13783,#4813,#4814);
#4040=DIRECTION('axis',(0.,0.,1.));
#4041=DIRECTION('refdir',(1.,0.,0.));
#4042=DIRECTION('axis',(0.,0.,1.));
#4043=DIRECTION('refdir',(1.,0.,0.));
#4044=DIRECTION('axis',(0.,0.,1.));
#4045=DIRECTION('refdir',(1.,0.,0.));
#4046=DIRECTION('center_axis',(-1.,0.,0.));
#4047=DIRECTION('ref_axis',(0.,1.,0.));
#4048=DIRECTION('center_axis',(-1.,0.,0.));
#4049=DIRECTION('ref_axis',(0.,1.,0.));
#4050=DIRECTION('',(-1.,0.,0.));
#4051=DIRECTION('center_axis',(-1.,0.,0.));
#4052=DIRECTION('ref_axis',(0.,1.,0.));
#4053=DIRECTION('center_axis',(-1.,0.,0.));
#4054=DIRECTION('ref_axis',(0.,1.,0.));
#4055=DIRECTION('center_axis',(-1.,0.,0.));
#4056=DIRECTION('ref_axis',(0.,1.,0.));
#4057=DIRECTION('center_axis',(-1.,0.,0.));
#4058=DIRECTION('ref_axis',(0.,1.,0.));
#4059=DIRECTION('',(-1.,0.,0.));
#4060=DIRECTION('center_axis',(-1.,0.,0.));
#4061=DIRECTION('ref_axis',(0.,1.,0.));
#4062=DIRECTION('center_axis',(-1.,0.,0.));
#4063=DIRECTION('ref_axis',(0.,1.,0.));
#4064=DIRECTION('center_axis',(1.,0.,0.));
#4065=DIRECTION('ref_axis',(0.,-1.,0.));
#4066=DIRECTION('center_axis',(1.,0.,0.));
#4067=DIRECTION('ref_axis',(0.,-1.,0.));
#4068=DIRECTION('',(1.,0.,0.));
#4069=DIRECTION('center_axis',(-1.,0.,0.));
#4070=DIRECTION('ref_axis',(0.,-1.,0.));
#4071=DIRECTION('center_axis',(1.,0.,0.));
#4072=DIRECTION('ref_axis',(0.,-1.,0.));
#4073=DIRECTION('center_axis',(1.,0.,0.));
#4074=DIRECTION('ref_axis',(0.,-1.,0.));
#4075=DIRECTION('',(1.,0.,0.));
#4076=DIRECTION('center_axis',(-1.,0.,0.));
#4077=DIRECTION('ref_axis',(0.,-1.,0.));
#4078=DIRECTION('center_axis',(1.,0.,0.));
#4079=DIRECTION('ref_axis',(0.,-1.,0.));
#4080=DIRECTION('center_axis',(1.,0.,0.));
#4081=DIRECTION('ref_axis',(0.,-1.,0.));
#4082=DIRECTION('',(1.,0.,0.));
#4083=DIRECTION('center_axis',(-1.,0.,0.));
#4084=DIRECTION('ref_axis',(0.,-1.,0.));
#4085=DIRECTION('center_axis',(1.,0.,0.));
#4086=DIRECTION('ref_axis',(0.,-1.,0.));
#4087=DIRECTION('center_axis',(1.,0.,0.));
#4088=DIRECTION('ref_axis',(0.,-1.,0.));
#4089=DIRECTION('',(1.,0.,0.));
#4090=DIRECTION('center_axis',(-1.,0.,0.));
#4091=DIRECTION('ref_axis',(0.,-1.,0.));
#4092=DIRECTION('center_axis',(1.,0.,0.));
#4093=DIRECTION('ref_axis',(0.,-1.,0.));
#4094=DIRECTION('center_axis',(1.,0.,0.));
#4095=DIRECTION('ref_axis',(0.,-1.,0.));
#4096=DIRECTION('',(1.,0.,0.));
#4097=DIRECTION('center_axis',(-1.,0.,0.));
#4098=DIRECTION('ref_axis',(0.,-1.,0.));
#4099=DIRECTION('center_axis',(1.,0.,0.));
#4100=DIRECTION('ref_axis',(0.,-1.,0.));
#4101=DIRECTION('center_axis',(1.,0.,0.));
#4102=DIRECTION('ref_axis',(0.,-1.,0.));
#4103=DIRECTION('',(1.,0.,0.));
#4104=DIRECTION('center_axis',(-1.,0.,0.));
#4105=DIRECTION('ref_axis',(0.,-1.,0.));
#4106=DIRECTION('center_axis',(0.,1.,0.));
#4107=DIRECTION('ref_axis',(-1.,0.,0.));
#4108=DIRECTION('',(-1.,0.,0.));
#4109=DIRECTION('',(0.,0.,1.));
#4110=DIRECTION('',(-1.,0.,0.));
#4111=DIRECTION('',(0.,0.,1.));
#4112=DIRECTION('center_axis',(1.,0.,0.));
#4113=DIRECTION('ref_axis',(0.,1.,0.));
#4114=DIRECTION('',(0.,1.,0.));
#4115=DIRECTION('',(0.,1.,0.));
#4116=DIRECTION('',(0.,0.,1.));
#4117=DIRECTION('center_axis',(0.,-1.,0.));
#4118=DIRECTION('ref_axis',(1.,0.,0.));
#4119=DIRECTION('',(1.,0.,0.));
#4120=DIRECTION('',(1.,0.,0.));
#4121=DIRECTION('',(0.,0.,1.));
#4122=DIRECTION('center_axis',(-1.,0.,0.));
#4123=DIRECTION('ref_axis',(0.,-1.,0.));
#4124=DIRECTION('',(0.,-1.,0.));
#4125=DIRECTION('',(0.,-1.,0.));
#4126=DIRECTION('center_axis',(0.,0.,1.));
#4127=DIRECTION('ref_axis',(1.,0.,0.));
#4128=DIRECTION('center_axis',(0.,0.,1.));
#4129=DIRECTION('ref_axis',(1.,0.,0.));
#4130=DIRECTION('axis',(0.,0.,1.));
#4131=DIRECTION('refdir',(1.,0.,0.));
#4132=DIRECTION('center_axis',(1.,0.,0.));
#4133=DIRECTION('ref_axis',(0.,-1.,0.));
#4134=DIRECTION('',(1.,0.,0.));
#4135=DIRECTION('center_axis',(-1.,0.,0.));
#4136=DIRECTION('ref_axis',(0.,-1.,0.));
#4137=DIRECTION('',(1.,0.,0.));
#4138=DIRECTION('center_axis',(-1.,0.,0.));
#4139=DIRECTION('ref_axis',(0.,-1.,0.));
#4140=DIRECTION('center_axis',(1.,0.,0.));
#4141=DIRECTION('ref_axis',(0.,-1.,0.));
#4142=DIRECTION('',(1.,0.,0.));
#4143=DIRECTION('center_axis',(1.,0.,0.));
#4144=DIRECTION('ref_axis',(0.,-1.,0.));
#4145=DIRECTION('',(1.,0.,0.));
#4146=DIRECTION('center_axis',(1.,0.,0.));
#4147=DIRECTION('ref_axis',(0.,-1.,0.));
#4148=DIRECTION('',(1.,0.,0.));
#4149=DIRECTION('center_axis',(1.,0.,0.));
#4150=DIRECTION('ref_axis',(0.,-1.,0.));
#4151=DIRECTION('',(1.,0.,0.));
#4152=DIRECTION('center_axis',(1.,0.,0.));
#4153=DIRECTION('ref_axis',(0.,-1.,0.));
#4154=DIRECTION('',(1.,0.,0.));
#4155=DIRECTION('center_axis',(1.,0.,0.));
#4156=DIRECTION('ref_axis',(0.,-1.,0.));
#4157=DIRECTION('',(1.,0.,0.));
#4158=DIRECTION('center_axis',(1.,0.,0.));
#4159=DIRECTION('ref_axis',(0.,-1.,0.));
#4160=DIRECTION('',(1.,0.,0.));
#4161=DIRECTION('center_axis',(1.,0.,0.));
#4162=DIRECTION('ref_axis',(0.,-1.,0.));
#4163=DIRECTION('',(1.,0.,0.));
#4164=DIRECTION('center_axis',(1.,0.,0.));
#4165=DIRECTION('ref_axis',(0.,-1.,0.));
#4166=DIRECTION('',(1.,0.,0.));
#4167=DIRECTION('center_axis',(1.,0.,0.));
#4168=DIRECTION('ref_axis',(0.,-1.,0.));
#4169=DIRECTION('',(1.,0.,0.));
#4170=DIRECTION('center_axis',(1.,0.,0.));
#4171=DIRECTION('ref_axis',(0.,-1.,0.));
#4172=DIRECTION('',(1.,0.,0.));
#4173=DIRECTION('center_axis',(1.,0.,0.));
#4174=DIRECTION('ref_axis',(0.,-0.939363391024623,-0.342923343624668));
#4175=DIRECTION('',(1.,0.,0.));
#4176=DIRECTION('center_axis',(1.,0.,0.));
#4177=DIRECTION('ref_axis',(0.,-1.,0.));
#4178=DIRECTION('center_axis',(1.,0.,0.));
#4179=DIRECTION('ref_axis',(0.,-0.130100013837605,0.991500875642304));
#4180=DIRECTION('',(1.,-1.22464679914735E-16,-9.41444059745064E-30));
#4181=DIRECTION('center_axis',(-1.,0.,0.));
#4182=DIRECTION('ref_axis',(0.,-1.,-7.67522767067882E-14));
#4183=DIRECTION('center_axis',(1.,0.,0.));
#4184=DIRECTION('ref_axis',(0.,-1.,-7.67522767067882E-14));
#4185=DIRECTION('',(1.,-1.22464679914735E-16,-9.41444059745064E-30));
#4186=DIRECTION('center_axis',(1.,0.,0.));
#4187=DIRECTION('ref_axis',(0.,-1.,-7.67522767067882E-14));
#4188=DIRECTION('',(1.,-1.22464679914735E-16,-9.41444059745064E-30));
#4189=DIRECTION('center_axis',(1.,0.,0.));
#4190=DIRECTION('ref_axis',(0.,-1.,-7.67522767067882E-14));
#4191=DIRECTION('',(1.,-1.22464679914735E-16,-9.41444059745064E-30));
#4192=DIRECTION('center_axis',(1.,0.,0.));
#4193=DIRECTION('ref_axis',(0.,-1.,-7.67522767067882E-14));
#4194=DIRECTION('',(1.,-1.22464679914735E-16,-9.41444059745064E-30));
#4195=DIRECTION('center_axis',(1.,0.,0.));
#4196=DIRECTION('ref_axis',(0.,-1.,-7.67522767067882E-14));
#4197=DIRECTION('',(1.,-1.22464679914735E-16,-9.41444059745064E-30));
#4198=DIRECTION('center_axis',(1.,0.,0.));
#4199=DIRECTION('ref_axis',(0.,-1.,-7.67522767067882E-14));
#4200=DIRECTION('',(1.,-1.22464679914735E-16,-9.41444059745064E-30));
#4201=DIRECTION('center_axis',(1.,0.,0.));
#4202=DIRECTION('ref_axis',(0.,-1.,-7.67522767067882E-14));
#4203=DIRECTION('',(1.,-1.22464679914735E-16,-9.41444059745064E-30));
#4204=DIRECTION('center_axis',(1.,0.,0.));
#4205=DIRECTION('ref_axis',(0.,-1.,-7.67522767067882E-14));
#4206=DIRECTION('',(1.,-1.22464679914735E-16,-9.41444059745064E-30));
#4207=DIRECTION('center_axis',(1.,0.,0.));
#4208=DIRECTION('ref_axis',(0.,-1.,-7.67522767067882E-14));
#4209=DIRECTION('',(1.,-1.22464679914735E-16,-9.41444059745064E-30));
#4210=DIRECTION('center_axis',(1.,0.,0.));
#4211=DIRECTION('ref_axis',(0.,-1.,-7.67522767067882E-14));
#4212=DIRECTION('',(1.,-1.22464679914735E-16,-9.41444059745064E-30));
#4213=DIRECTION('center_axis',(1.,0.,0.));
#4214=DIRECTION('ref_axis',(0.,-1.,-7.67522767067882E-14));
#4215=DIRECTION('',(1.,-1.22464679914735E-16,-9.41444059745064E-30));
#4216=DIRECTION('center_axis',(1.,0.,0.));
#4217=DIRECTION('ref_axis',(0.,-1.,-7.67522767067882E-14));
#4218=DIRECTION('',(1.,-1.22464679914735E-16,-9.41444059745064E-30));
#4219=DIRECTION('center_axis',(1.,0.,0.));
#4220=DIRECTION('ref_axis',(0.,0.609130550517291,-0.793069966917486));
#4221=DIRECTION('',(1.,-1.22464679914735E-16,-9.41444059745064E-30));
#4222=DIRECTION('center_axis',(1.,0.,0.));
#4223=DIRECTION('ref_axis',(0.,-1.,-7.67522767067882E-14));
#4224=DIRECTION('center_axis',(1.,0.,0.));
#4225=DIRECTION('ref_axis',(0.,-1.,0.));
#4226=DIRECTION('',(1.,0.,0.));
#4227=DIRECTION('center_axis',(-1.,0.,0.));
#4228=DIRECTION('ref_axis',(0.,-1.,0.));
#4229=DIRECTION('',(1.,0.,0.));
#4230=DIRECTION('center_axis',(-1.,0.,0.));
#4231=DIRECTION('ref_axis',(0.,-1.,0.));
#4232=DIRECTION('center_axis',(1.,0.,0.));
#4233=DIRECTION('ref_axis',(0.,-1.,0.));
#4234=DIRECTION('',(1.,0.,0.));
#4235=DIRECTION('center_axis',(1.,0.,0.));
#4236=DIRECTION('ref_axis',(0.,-1.,0.));
#4237=DIRECTION('',(1.,0.,0.));
#4238=DIRECTION('center_axis',(1.,0.,0.));
#4239=DIRECTION('ref_axis',(0.,-1.,0.));
#4240=DIRECTION('',(1.,0.,0.));
#4241=DIRECTION('center_axis',(1.,0.,0.));
#4242=DIRECTION('ref_axis',(0.,-1.,0.));
#4243=DIRECTION('',(1.,0.,0.));
#4244=DIRECTION('center_axis',(1.,0.,0.));
#4245=DIRECTION('ref_axis',(0.,-1.,0.));
#4246=DIRECTION('',(1.,0.,0.));
#4247=DIRECTION('center_axis',(1.,0.,0.));
#4248=DIRECTION('ref_axis',(0.,-1.,0.));
#4249=DIRECTION('',(1.,0.,0.));
#4250=DIRECTION('center_axis',(1.,0.,0.));
#4251=DIRECTION('ref_axis',(0.,-1.,0.));
#4252=DIRECTION('',(1.,0.,0.));
#4253=DIRECTION('center_axis',(1.,0.,0.));
#4254=DIRECTION('ref_axis',(0.,-1.,0.));
#4255=DIRECTION('',(1.,0.,0.));
#4256=DIRECTION('center_axis',(1.,0.,0.));
#4257=DIRECTION('ref_axis',(0.,-1.,0.));
#4258=DIRECTION('',(1.,0.,0.));
#4259=DIRECTION('center_axis',(1.,0.,0.));
#4260=DIRECTION('ref_axis',(0.,-1.,0.));
#4261=DIRECTION('',(1.,0.,0.));
#4262=DIRECTION('center_axis',(1.,0.,0.));
#4263=DIRECTION('ref_axis',(0.,-1.,0.));
#4264=DIRECTION('',(1.,0.,0.));
#4265=DIRECTION('center_axis',(1.,0.,0.));
#4266=DIRECTION('ref_axis',(0.,-0.939363407112957,-0.342923299554197));
#4267=DIRECTION('',(1.,0.,0.));
#4268=DIRECTION('center_axis',(1.,0.,0.));
#4269=DIRECTION('ref_axis',(0.,-1.,0.));
#4270=DIRECTION('center_axis',(1.,0.,0.));
#4271=DIRECTION('ref_axis',(0.,-0.130100058958222,0.991500869721791));
#4272=DIRECTION('',(1.,-1.22464679914735E-16,-9.41427121902906E-30));
#4273=DIRECTION('center_axis',(-1.,0.,0.));
#4274=DIRECTION('ref_axis',(0.,-1.,-7.67508936270162E-14));
#4275=DIRECTION('center_axis',(1.,0.,0.));
#4276=DIRECTION('ref_axis',(0.,-1.,-7.67508936270162E-14));
#4277=DIRECTION('',(1.,-1.22464679914735E-16,-9.41427121902906E-30));
#4278=DIRECTION('center_axis',(1.,0.,0.));
#4279=DIRECTION('ref_axis',(0.,-1.,-7.67508936270162E-14));
#4280=DIRECTION('',(1.,-1.22464679914735E-16,-9.41427121902906E-30));
#4281=DIRECTION('center_axis',(1.,0.,0.));
#4282=DIRECTION('ref_axis',(0.,-1.,-7.67508936270162E-14));
#4283=DIRECTION('',(1.,-1.22464679914735E-16,-9.41427121902906E-30));
#4284=DIRECTION('center_axis',(1.,0.,0.));
#4285=DIRECTION('ref_axis',(0.,-1.,-7.67508936270162E-14));
#4286=DIRECTION('',(1.,-1.22464679914735E-16,-9.41427121902906E-30));
#4287=DIRECTION('center_axis',(1.,0.,0.));
#4288=DIRECTION('ref_axis',(0.,-1.,-7.67508936270162E-14));
#4289=DIRECTION('',(1.,-1.22464679914735E-16,-9.41427121902906E-30));
#4290=DIRECTION('center_axis',(1.,0.,0.));
#4291=DIRECTION('ref_axis',(0.,-1.,-7.67508936270162E-14));
#4292=DIRECTION('',(1.,-1.22464679914735E-16,-9.41427121902906E-30));
#4293=DIRECTION('center_axis',(1.,0.,0.));
#4294=DIRECTION('ref_axis',(0.,-1.,-7.67508936270162E-14));
#4295=DIRECTION('',(1.,-1.22464679914735E-16,-9.41427121902906E-30));
#4296=DIRECTION('center_axis',(1.,0.,0.));
#4297=DIRECTION('ref_axis',(0.,-1.,-7.67508936270162E-14));
#4298=DIRECTION('',(1.,-1.22464679914735E-16,-9.41427121902906E-30));
#4299=DIRECTION('center_axis',(1.,0.,0.));
#4300=DIRECTION('ref_axis',(0.,-1.,-7.67508936270162E-14));
#4301=DIRECTION('',(1.,-1.22464679914735E-16,-9.41427121902906E-30));
#4302=DIRECTION('center_axis',(1.,0.,0.));
#4303=DIRECTION('ref_axis',(0.,-1.,-7.67508936270162E-14));
#4304=DIRECTION('',(1.,-1.22464679914735E-16,-9.41427121902906E-30));
#4305=DIRECTION('center_axis',(1.,0.,0.));
#4306=DIRECTION('ref_axis',(0.,-1.,-7.67508936270162E-14));
#4307=DIRECTION('',(1.,-1.22464679914735E-16,-9.41427121902906E-30));
#4308=DIRECTION('center_axis',(1.,0.,0.));
#4309=DIRECTION('ref_axis',(0.,-1.,-7.67508936270162E-14));
#4310=DIRECTION('',(1.,-1.22464679914735E-16,-9.41427121902906E-30));
#4311=DIRECTION('center_axis',(1.,0.,0.));
#4312=DIRECTION('ref_axis',(0.,0.609130584443187,-0.793069940860137));
#4313=DIRECTION('',(1.,-1.22464679914735E-16,-9.41427121902906E-30));
#4314=DIRECTION('center_axis',(1.,0.,0.));
#4315=DIRECTION('ref_axis',(0.,-1.,-7.67508936270162E-14));
#4316=DIRECTION('center_axis',(1.,0.,0.));
#4317=DIRECTION('ref_axis',(0.,-1.,0.));
#4318=DIRECTION('center_axis',(1.,0.,0.));
#4319=DIRECTION('ref_axis',(0.,-1.,0.));
#4320=DIRECTION('',(1.,0.,0.));
#4321=DIRECTION('center_axis',(1.,0.,0.));
#4322=DIRECTION('ref_axis',(0.,-1.,0.));
#4323=DIRECTION('center_axis',(1.,0.,0.));
#4324=DIRECTION('ref_axis',(0.,-1.,0.));
#4325=DIRECTION('center_axis',(1.,0.,0.));
#4326=DIRECTION('ref_axis',(0.,-1.,0.));
#4327=DIRECTION('center_axis',(1.,0.,0.));
#4328=DIRECTION('ref_axis',(0.,-1.,0.));
#4329=DIRECTION('',(1.,0.,0.));
#4330=DIRECTION('center_axis',(1.,0.,0.));
#4331=DIRECTION('ref_axis',(0.,-1.,0.));
#4332=DIRECTION('center_axis',(1.,0.,0.));
#4333=DIRECTION('ref_axis',(0.,-1.,0.));
#4334=DIRECTION('center_axis',(1.,0.,0.));
#4335=DIRECTION('ref_axis',(0.,0.,-1.));
#4336=DIRECTION('center_axis',(1.,0.,0.));
#4337=DIRECTION('ref_axis',(0.,-1.,-7.67508936270162E-14));
#4338=DIRECTION('center_axis',(1.,0.,0.));
#4339=DIRECTION('ref_axis',(0.,-1.,0.));
#4340=DIRECTION('center_axis',(1.,0.,0.));
#4341=DIRECTION('ref_axis',(0.,0.,-1.));
#4342=DIRECTION('center_axis',(1.,0.,0.));
#4343=DIRECTION('ref_axis',(0.,-1.,-7.67522767067882E-14));
#4344=DIRECTION('center_axis',(1.,0.,0.));
#4345=DIRECTION('ref_axis',(0.,-1.,0.));
#4346=DIRECTION('center_axis',(1.,0.,0.));
#4347=DIRECTION('ref_axis',(0.,-1.,0.));
#4348=DIRECTION('center_axis',(1.,0.,0.));
#4349=DIRECTION('ref_axis',(0.,-1.,0.));
#4350=DIRECTION('center_axis',(0.,1.,0.));
#4351=DIRECTION('ref_axis',(-1.,0.,0.));
#4352=DIRECTION('',(-1.,0.,0.));
#4353=DIRECTION('',(0.,0.,1.));
#4354=DIRECTION('',(-1.,0.,0.));
#4355=DIRECTION('',(0.,0.,1.));
#4356=DIRECTION('center_axis',(0.,0.,1.));
#4357=DIRECTION('ref_axis',(0.,-1.,0.));
#4358=DIRECTION('center_axis',(0.,0.,-1.));
#4359=DIRECTION('ref_axis',(0.,-1.,0.));
#4360=DIRECTION('center_axis',(0.,0.,-1.));
#4361=DIRECTION('ref_axis',(0.,-1.,0.));
#4362=DIRECTION('',(0.,0.,1.));
#4363=DIRECTION('center_axis',(-1.,0.,0.));
#4364=DIRECTION('ref_axis',(0.,-1.,0.));
#4365=DIRECTION('',(0.,-1.,0.));
#4366=DIRECTION('',(0.,-1.,0.));
#4367=DIRECTION('',(0.,0.,1.));
#4368=DIRECTION('center_axis',(0.,0.,1.));
#4369=DIRECTION('ref_axis',(1.,-3.33066907387548E-15,0.));
#4370=DIRECTION('center_axis',(0.,0.,-1.));
#4371=DIRECTION('ref_axis',(1.,-3.33066907387548E-15,0.));
#4372=DIRECTION('center_axis',(0.,0.,-1.));
#4373=DIRECTION('ref_axis',(1.,-3.33066907387548E-15,0.));
#4374=DIRECTION('',(0.,0.,1.));
#4375=DIRECTION('center_axis',(0.,-1.,0.));
#4376=DIRECTION('ref_axis',(1.,0.,0.));
#4377=DIRECTION('',(1.,0.,0.));
#4378=DIRECTION('',(1.,0.,0.));
#4379=DIRECTION('',(0.,0.,1.));
#4380=DIRECTION('center_axis',(0.,0.,1.));
#4381=DIRECTION('ref_axis',(2.22044604925032E-15,1.,0.));
#4382=DIRECTION('center_axis',(0.,0.,-1.));
#4383=DIRECTION('ref_axis',(2.22044604925032E-15,1.,0.));
#4384=DIRECTION('center_axis',(0.,0.,-1.));
#4385=DIRECTION('ref_axis',(2.22044604925032E-15,1.,0.));
#4386=DIRECTION('',(0.,0.,1.));
#4387=DIRECTION('center_axis',(1.,0.,0.));
#4388=DIRECTION('ref_axis',(0.,1.,0.));
#4389=DIRECTION('',(0.,1.,0.));
#4390=DIRECTION('',(0.,1.,0.));
#4391=DIRECTION('',(0.,0.,1.));
#4392=DIRECTION('center_axis',(0.,0.,1.));
#4393=DIRECTION('ref_axis',(-1.,1.66533453693774E-15,0.));
#4394=DIRECTION('center_axis',(0.,0.,-1.));
#4395=DIRECTION('ref_axis',(-1.,1.66533453693774E-15,0.));
#4396=DIRECTION('center_axis',(0.,0.,-1.));
#4397=DIRECTION('ref_axis',(-1.,1.66533453693774E-15,0.));
#4398=DIRECTION('center_axis',(0.,0.,1.));
#4399=DIRECTION('ref_axis',(-1.,0.,0.));
#4400=DIRECTION('center_axis',(0.,0.,1.));
#4401=DIRECTION('ref_axis',(-1.,0.,0.));
#4402=DIRECTION('',(0.,0.,1.));
#4403=DIRECTION('center_axis',(0.,0.,-1.));
#4404=DIRECTION('ref_axis',(-1.,0.,0.));
#4405=DIRECTION('',(0.,0.,1.));
#4406=DIRECTION('center_axis',(0.,1.,0.));
#4407=DIRECTION('ref_axis',(-1.,0.,0.));
#4408=DIRECTION('',(-1.,0.,0.));
#4409=DIRECTION('',(-1.,0.,0.));
#4410=DIRECTION('',(0.,0.,1.));
#4411=DIRECTION('center_axis',(0.,0.,1.));
#4412=DIRECTION('ref_axis',(4.44089209850061E-15,-1.,0.));
#4413=DIRECTION('center_axis',(0.,0.,1.));
#4414=DIRECTION('ref_axis',(4.44089209850061E-15,-1.,0.));
#4415=DIRECTION('center_axis',(0.,0.,-1.));
#4416=DIRECTION('ref_axis',(4.44089209850061E-15,-1.,0.));
#4417=DIRECTION('',(0.,0.,1.));
#4418=DIRECTION('center_axis',(-1.,0.,0.));
#4419=DIRECTION('ref_axis',(0.,-1.,0.));
#4420=DIRECTION('',(0.,-1.,0.));
#4421=DIRECTION('',(0.,-1.,0.));
#4422=DIRECTION('',(0.,0.,1.));
#4423=DIRECTION('center_axis',(0.,1.,0.));
#4424=DIRECTION('ref_axis',(-1.,0.,0.));
#4425=DIRECTION('',(-1.,0.,0.));
#4426=DIRECTION('',(-1.,0.,0.));
#4427=DIRECTION('',(0.,0.,1.));
#4428=DIRECTION('center_axis',(1.,0.,0.));
#4429=DIRECTION('ref_axis',(0.,1.,0.));
#4430=DIRECTION('',(0.,1.,0.));
#4431=DIRECTION('',(0.,1.,0.));
#4432=DIRECTION('',(0.,0.,1.));
#4433=DIRECTION('center_axis',(0.,-1.,0.));
#4434=DIRECTION('ref_axis',(1.,0.,0.));
#4435=DIRECTION('',(1.,0.,0.));
#4436=DIRECTION('',(1.,0.,0.));
#4437=DIRECTION('',(0.,0.,1.));
#4438=DIRECTION('center_axis',(-1.,0.,0.));
#4439=DIRECTION('ref_axis',(0.,-1.,0.));
#4440=DIRECTION('',(0.,-1.,0.));
#4441=DIRECTION('',(0.,-1.,0.));
#4442=DIRECTION('',(0.,0.,1.));
#4443=DIRECTION('center_axis',(0.,0.,1.));
#4444=DIRECTION('ref_axis',(1.,4.4408920985006E-15,0.));
#4445=DIRECTION('center_axis',(0.,0.,1.));
#4446=DIRECTION('ref_axis',(1.,4.4408920985006E-15,0.));
#4447=DIRECTION('center_axis',(0.,0.,-1.));
#4448=DIRECTION('ref_axis',(1.,4.4408920985006E-15,0.));
#4449=DIRECTION('',(0.,0.,1.));
#4450=DIRECTION('center_axis',(0.,-1.,0.));
#4451=DIRECTION('ref_axis',(1.,0.,0.));
#4452=DIRECTION('',(1.,0.,0.));
#4453=DIRECTION('',(1.,0.,0.));
#4454=DIRECTION('',(0.,0.,1.));
#4455=DIRECTION('center_axis',(0.,0.,1.));
#4456=DIRECTION('ref_axis',(0.,1.,0.));
#4457=DIRECTION('center_axis',(0.,0.,1.));
#4458=DIRECTION('ref_axis',(0.,1.,0.));
#4459=DIRECTION('center_axis',(0.,0.,-1.));
#4460=DIRECTION('ref_axis',(0.,1.,0.));
#4461=DIRECTION('',(0.,0.,1.));
#4462=DIRECTION('center_axis',(1.,0.,0.));
#4463=DIRECTION('ref_axis',(0.,1.,0.));
#4464=DIRECTION('',(0.,1.,0.));
#4465=DIRECTION('',(0.,1.,0.));
#4466=DIRECTION('',(0.,0.,1.));
#4467=DIRECTION('center_axis',(0.,-1.,0.));
#4468=DIRECTION('ref_axis',(1.,0.,0.));
#4469=DIRECTION('',(1.,0.,0.));
#4470=DIRECTION('',(1.,0.,0.));
#4471=DIRECTION('',(0.,0.,1.));
#4472=DIRECTION('center_axis',(-1.,0.,0.));
#4473=DIRECTION('ref_axis',(0.,-1.,0.));
#4474=DIRECTION('',(0.,-1.,0.));
#4475=DIRECTION('',(0.,-1.,0.));
#4476=DIRECTION('',(0.,0.,1.));
#4477=DIRECTION('center_axis',(0.,1.,0.));
#4478=DIRECTION('ref_axis',(-1.,0.,0.));
#4479=DIRECTION('',(-1.,0.,0.));
#4480=DIRECTION('',(-1.,0.,0.));
#4481=DIRECTION('',(0.,0.,1.));
#4482=DIRECTION('center_axis',(1.,0.,0.));
#4483=DIRECTION('ref_axis',(0.,1.,0.));
#4484=DIRECTION('',(0.,1.,0.));
#4485=DIRECTION('',(0.,1.,0.));
#4486=DIRECTION('center_axis',(0.,0.,1.));
#4487=DIRECTION('ref_axis',(1.,0.,0.));
#4488=DIRECTION('center_axis',(0.,0.,1.));
#4489=DIRECTION('ref_axis',(1.,0.,0.));
#4490=DIRECTION('axis',(0.,0.,1.));
#4491=DIRECTION('refdir',(1.,0.,0.));
#4492=DIRECTION('center_axis',(0.,1.,0.));
#4493=DIRECTION('ref_axis',(-1.,0.,0.));
#4494=DIRECTION('',(-1.,0.,0.));
#4495=DIRECTION('',(0.,0.,1.));
#4496=DIRECTION('',(-1.,0.,0.));
#4497=DIRECTION('',(0.,0.,1.));
#4498=DIRECTION('center_axis',(1.,0.,0.));
#4499=DIRECTION('ref_axis',(0.,1.,0.));
#4500=DIRECTION('',(0.,1.,0.));
#4501=DIRECTION('',(0.,1.,0.));
#4502=DIRECTION('',(0.,0.,1.));
#4503=DIRECTION('center_axis',(0.,-1.,0.));
#4504=DIRECTION('ref_axis',(1.,0.,0.));
#4505=DIRECTION('',(1.,0.,0.));
#4506=DIRECTION('',(1.,0.,0.));
#4507=DIRECTION('',(0.,0.,1.));
#4508=DIRECTION('center_axis',(-1.,0.,0.));
#4509=DIRECTION('ref_axis',(0.,-1.,0.));
#4510=DIRECTION('',(0.,-1.,0.));
#4511=DIRECTION('',(0.,-1.,0.));
#4512=DIRECTION('center_axis',(0.,0.,1.));
#4513=DIRECTION('ref_axis',(1.,0.,0.));
#4514=DIRECTION('center_axis',(0.,0.,1.));
#4515=DIRECTION('ref_axis',(1.,0.,0.));
#4516=DIRECTION('axis',(0.,0.,1.));
#4517=DIRECTION('refdir',(1.,0.,0.));
#4518=DIRECTION('center_axis',(0.,0.,1.));
#4519=DIRECTION('ref_axis',(1.,0.,0.));
#4520=DIRECTION('center_axis',(0.,0.,-1.));
#4521=DIRECTION('ref_axis',(1.,0.,0.));
#4522=DIRECTION('',(0.,0.,-1.));
#4523=DIRECTION('center_axis',(0.,0.,-1.));
#4524=DIRECTION('ref_axis',(1.,0.,0.));
#4525=DIRECTION('center_axis',(0.,0.,1.));
#4526=DIRECTION('ref_axis',(1.,0.,0.));
#4527=DIRECTION('center_axis',(0.,0.,1.));
#4528=DIRECTION('ref_axis',(1.,0.,0.));
#4529=DIRECTION('',(0.,0.,-1.));
#4530=DIRECTION('center_axis',(0.,0.,1.));
#4531=DIRECTION('ref_axis',(1.,0.,0.));
#4532=DIRECTION('center_axis',(0.,0.,1.));
#4533=DIRECTION('ref_axis',(1.,0.,0.));
#4534=DIRECTION('center_axis',(0.,0.,1.));
#4535=DIRECTION('ref_axis',(1.,0.,0.));
#4536=DIRECTION('axis',(0.,0.,1.));
#4537=DIRECTION('refdir',(1.,0.,0.));
#4538=DIRECTION('center_axis',(0.,0.,1.));
#4539=DIRECTION('ref_axis',(1.,0.,0.));
#4540=DIRECTION('',(0.,0.,-1.));
#4541=DIRECTION('center_axis',(0.,0.,-1.));
#4542=DIRECTION('ref_axis',(1.,0.,0.));
#4543=DIRECTION('center_axis',(0.,0.,1.));
#4544=DIRECTION('ref_axis',(1.,0.,0.));
#4545=DIRECTION('',(0.,0.,-1.));
#4546=DIRECTION('center_axis',(0.,0.,1.));
#4547=DIRECTION('ref_axis',(1.,0.,0.));
#4548=DIRECTION('',(0.,0.,-1.));
#4549=DIRECTION('center_axis',(0.,0.,1.));
#4550=DIRECTION('ref_axis',(1.,0.,0.));
#4551=DIRECTION('',(0.,0.,-1.));
#4552=DIRECTION('center_axis',(0.,0.,1.));
#4553=DIRECTION('ref_axis',(1.,0.,0.));
#4554=DIRECTION('',(0.,0.,-1.));
#4555=DIRECTION('center_axis',(0.,0.,1.));
#4556=DIRECTION('ref_axis',(1.,0.,0.));
#4557=DIRECTION('',(0.,0.,-1.));
#4558=DIRECTION('center_axis',(0.,0.,1.));
#4559=DIRECTION('ref_axis',(1.,0.,0.));
#4560=DIRECTION('',(0.,0.,-1.));
#4561=DIRECTION('center_axis',(0.,0.,1.));
#4562=DIRECTION('ref_axis',(1.,0.,0.));
#4563=DIRECTION('',(0.,0.,-1.));
#4564=DIRECTION('center_axis',(0.,0.,1.));
#4565=DIRECTION('ref_axis',(1.,0.,0.));
#4566=DIRECTION('',(0.,0.,-1.));
#4567=DIRECTION('center_axis',(0.,0.,1.));
#4568=DIRECTION('ref_axis',(1.,0.,0.));
#4569=DIRECTION('',(0.,0.,-1.));
#4570=DIRECTION('center_axis',(0.,0.,1.));
#4571=DIRECTION('ref_axis',(1.,0.,0.));
#4572=DIRECTION('',(0.,0.,-1.));
#4573=DIRECTION('center_axis',(0.,0.,1.));
#4574=DIRECTION('ref_axis',(1.,0.,0.));
#4575=DIRECTION('',(0.,0.,-1.));
#4576=DIRECTION('center_axis',(0.,0.,1.));
#4577=DIRECTION('ref_axis',(1.,0.,0.));
#4578=DIRECTION('',(0.,0.,-1.));
#4579=DIRECTION('center_axis',(0.,0.,1.));
#4580=DIRECTION('ref_axis',(1.,0.,0.));
#4581=DIRECTION('',(0.,0.,-1.));
#4582=DIRECTION('center_axis',(0.,0.,1.));
#4583=DIRECTION('ref_axis',(1.,0.,0.));
#4584=DIRECTION('',(0.,0.,-1.));
#4585=DIRECTION('center_axis',(0.,0.,1.));
#4586=DIRECTION('ref_axis',(1.,0.,0.));
#4587=DIRECTION('',(0.,0.,-1.));
#4588=DIRECTION('center_axis',(0.,0.,1.));
#4589=DIRECTION('ref_axis',(1.,0.,0.));
#4590=DIRECTION('',(0.,0.,-1.));
#4591=DIRECTION('center_axis',(0.,0.,1.));
#4592=DIRECTION('ref_axis',(1.,0.,0.));
#4593=DIRECTION('',(0.,0.,-1.));
#4594=DIRECTION('center_axis',(0.,0.,1.));
#4595=DIRECTION('ref_axis',(1.,0.,0.));
#4596=DIRECTION('',(0.,0.,-1.));
#4597=DIRECTION('center_axis',(0.,0.,1.));
#4598=DIRECTION('ref_axis',(1.,0.,0.));
#4599=DIRECTION('',(0.,0.,-1.));
#4600=DIRECTION('center_axis',(0.,0.,1.));
#4601=DIRECTION('ref_axis',(1.,0.,0.));
#4602=DIRECTION('',(0.,0.,-1.));
#4603=DIRECTION('center_axis',(0.,0.,1.));
#4604=DIRECTION('ref_axis',(1.,0.,0.));
#4605=DIRECTION('',(0.,0.,-1.));
#4606=DIRECTION('center_axis',(0.,0.,1.));
#4607=DIRECTION('ref_axis',(1.,0.,0.));
#4608=DIRECTION('',(0.,0.,-1.));
#4609=DIRECTION('center_axis',(0.,0.,1.));
#4610=DIRECTION('ref_axis',(1.,0.,0.));
#4611=DIRECTION('',(0.,0.,-1.));
#4612=DIRECTION('center_axis',(0.,0.,1.));
#4613=DIRECTION('ref_axis',(1.,0.,0.));
#4614=DIRECTION('',(0.,0.,-1.));
#4615=DIRECTION('center_axis',(0.,0.,1.));
#4616=DIRECTION('ref_axis',(1.,0.,0.));
#4617=DIRECTION('',(0.,0.,-1.));
#4618=DIRECTION('center_axis',(0.,0.,1.));
#4619=DIRECTION('ref_axis',(1.,0.,0.));
#4620=DIRECTION('',(0.,0.,-1.));
#4621=DIRECTION('center_axis',(0.,0.,1.));
#4622=DIRECTION('ref_axis',(1.,0.,0.));
#4623=DIRECTION('',(0.,0.,-1.));
#4624=DIRECTION('center_axis',(0.,0.,1.));
#4625=DIRECTION('ref_axis',(1.,0.,0.));
#4626=DIRECTION('',(0.,0.,-1.));
#4627=DIRECTION('center_axis',(0.,0.,1.));
#4628=DIRECTION('ref_axis',(1.,0.,0.));
#4629=DIRECTION('',(0.,0.,-1.));
#4630=DIRECTION('center_axis',(0.,0.,1.));
#4631=DIRECTION('ref_axis',(0.99808566179124,-0.0618466791892788,0.));
#4632=DIRECTION('',(0.,0.,1.));
#4633=DIRECTION('center_axis',(0.,0.,-1.));
#4634=DIRECTION('ref_axis',(1.,-2.02644595590483E-13,0.));
#4635=DIRECTION('center_axis',(0.,0.,1.));
#4636=DIRECTION('ref_axis',(1.,-2.02644595590483E-13,0.));
#4637=DIRECTION('',(0.,0.,1.));
#4638=DIRECTION('center_axis',(0.,0.,1.));
#4639=DIRECTION('ref_axis',(1.,-2.02644595590483E-13,0.));
#4640=DIRECTION('',(0.,0.,1.));
#4641=DIRECTION('center_axis',(0.,0.,1.));
#4642=DIRECTION('ref_axis',(1.,-2.02644595590483E-13,0.));
#4643=DIRECTION('',(0.,0.,1.));
#4644=DIRECTION('center_axis',(0.,0.,1.));
#4645=DIRECTION('ref_axis',(1.,-2.02644595590483E-13,0.));
#4646=DIRECTION('',(0.,0.,1.));
#4647=DIRECTION('center_axis',(0.,0.,1.));
#4648=DIRECTION('ref_axis',(1.,-2.02644595590483E-13,0.));
#4649=DIRECTION('',(0.,0.,1.));
#4650=DIRECTION('center_axis',(0.,0.,1.));
#4651=DIRECTION('ref_axis',(1.,-2.02644595590483E-13,0.));
#4652=DIRECTION('',(0.,0.,1.));
#4653=DIRECTION('center_axis',(0.,0.,1.));
#4654=DIRECTION('ref_axis',(1.,-2.02644595590483E-13,0.));
#4655=DIRECTION('',(0.,0.,1.));
#4656=DIRECTION('center_axis',(0.,0.,1.));
#4657=DIRECTION('ref_axis',(1.,-2.02644595590483E-13,0.));
#4658=DIRECTION('',(0.,0.,1.));
#4659=DIRECTION('center_axis',(0.,0.,1.));
#4660=DIRECTION('ref_axis',(1.,-2.02644595590483E-13,0.));
#4661=DIRECTION('',(0.,0.,1.));
#4662=DIRECTION('center_axis',(0.,0.,1.));
#4663=DIRECTION('ref_axis',(1.,-2.02644595590483E-13,0.));
#4664=DIRECTION('',(0.,0.,1.));
#4665=DIRECTION('center_axis',(0.,0.,1.));
#4666=DIRECTION('ref_axis',(1.,-2.02644595590483E-13,0.));
#4667=DIRECTION('',(0.,0.,1.));
#4668=DIRECTION('center_axis',(0.,0.,1.));
#4669=DIRECTION('ref_axis',(1.,-2.02644595590483E-13,0.));
#4670=DIRECTION('',(0.,0.,1.));
#4671=DIRECTION('center_axis',(0.,0.,1.));
#4672=DIRECTION('ref_axis',(1.,-2.02644595590483E-13,0.));
#4673=DIRECTION('',(0.,0.,1.));
#4674=DIRECTION('center_axis',(0.,0.,1.));
#4675=DIRECTION('ref_axis',(1.,-2.02644595590483E-13,0.));
#4676=DIRECTION('',(0.,0.,1.));
#4677=DIRECTION('center_axis',(0.,0.,1.));
#4678=DIRECTION('ref_axis',(1.,-2.02644595590483E-13,0.));
#4679=DIRECTION('',(0.,0.,1.));
#4680=DIRECTION('center_axis',(0.,0.,1.));
#4681=DIRECTION('ref_axis',(1.,-2.02644595590483E-13,0.));
#4682=DIRECTION('',(0.,0.,1.));
#4683=DIRECTION('center_axis',(0.,0.,1.));
#4684=DIRECTION('ref_axis',(1.,-2.02644595590483E-13,0.));
#4685=DIRECTION('',(0.,0.,1.));
#4686=DIRECTION('center_axis',(0.,0.,1.));
#4687=DIRECTION('ref_axis',(1.,-2.02644595590483E-13,0.));
#4688=DIRECTION('',(0.,0.,1.));
#4689=DIRECTION('center_axis',(0.,0.,1.));
#4690=DIRECTION('ref_axis',(1.,-2.02644595590483E-13,0.));
#4691=DIRECTION('',(0.,0.,1.));
#4692=DIRECTION('center_axis',(0.,0.,1.));
#4693=DIRECTION('ref_axis',(1.,-2.02644595590483E-13,0.));
#4694=DIRECTION('',(0.,0.,1.));
#4695=DIRECTION('center_axis',(0.,0.,1.));
#4696=DIRECTION('ref_axis',(1.,-2.02644595590483E-13,0.));
#4697=DIRECTION('',(0.,0.,1.));
#4698=DIRECTION('center_axis',(0.,0.,1.));
#4699=DIRECTION('ref_axis',(1.,-2.02644595590483E-13,0.));
#4700=DIRECTION('',(0.,0.,1.));
#4701=DIRECTION('center_axis',(0.,0.,1.));
#4702=DIRECTION('ref_axis',(1.,-2.02644595590483E-13,0.));
#4703=DIRECTION('',(0.,0.,1.));
#4704=DIRECTION('center_axis',(0.,0.,1.));
#4705=DIRECTION('ref_axis',(1.,-2.02644595590483E-13,0.));
#4706=DIRECTION('',(0.,0.,1.));
#4707=DIRECTION('center_axis',(0.,0.,1.));
#4708=DIRECTION('ref_axis',(1.,-2.02644595590483E-13,0.));
#4709=DIRECTION('',(0.,0.,1.));
#4710=DIRECTION('center_axis',(0.,0.,1.));
#4711=DIRECTION('ref_axis',(1.,-2.02644595590483E-13,0.));
#4712=DIRECTION('',(0.,0.,1.));
#4713=DIRECTION('center_axis',(0.,0.,1.));
#4714=DIRECTION('ref_axis',(1.,-2.02644595590483E-13,0.));
#4715=DIRECTION('',(0.,0.,1.));
#4716=DIRECTION('center_axis',(0.,0.,1.));
#4717=DIRECTION('ref_axis',(1.,-2.02644595590483E-13,0.));
#4718=DIRECTION('',(0.,0.,1.));
#4719=DIRECTION('center_axis',(0.,0.,1.));
#4720=DIRECTION('ref_axis',(1.,-2.02644595590483E-13,0.));
#4721=DIRECTION('',(0.,0.,1.));
#4722=DIRECTION('center_axis',(0.,0.,-1.));
#4723=DIRECTION('ref_axis',(1.,0.,0.));
#4724=DIRECTION('center_axis',(0.,0.,-1.));
#4725=DIRECTION('ref_axis',(1.,0.,0.));
#4726=DIRECTION('',(0.707106781186547,8.65956056235493E-17,0.707106781186548));
#4727=DIRECTION('center_axis',(0.,0.,1.));
#4728=DIRECTION('ref_axis',(1.,0.,0.));
#4729=DIRECTION('center_axis',(0.,0.,1.));
#4730=DIRECTION('ref_axis',(1.,-2.02644595590483E-13,0.));
#4731=DIRECTION('center_axis',(0.,0.,-1.));
#4732=DIRECTION('ref_axis',(1.,-2.02644595590483E-13,0.));
#4733=DIRECTION('center_axis',(0.,0.,1.));
#4734=DIRECTION('ref_axis',(1.,0.,0.));
#4735=DIRECTION('center_axis',(-2.40370335797945E-16,-1.,0.));
#4736=DIRECTION('ref_axis',(1.,-2.40370335797945E-16,0.));
#4737=DIRECTION('',(1.,-2.40370335797945E-16,0.));
#4738=DIRECTION('',(0.,0.,1.));
#4739=DIRECTION('',(1.,-2.40370335797945E-16,0.));
#4740=DIRECTION('',(0.,0.,1.));
#4741=DIRECTION('center_axis',(-0.866025403784439,-0.5,0.));
#4742=DIRECTION('ref_axis',(0.5,-0.866025403784439,0.));
#4743=DIRECTION('',(0.5,-0.866025403784439,0.));
#4744=DIRECTION('',(0.,0.,1.));
#4745=DIRECTION('',(0.5,-0.866025403784439,0.));
#4746=DIRECTION('center_axis',(-0.866025403784439,0.5,0.));
#4747=DIRECTION('ref_axis',(-0.5,-0.866025403784439,0.));
#4748=DIRECTION('',(-0.5,-0.866025403784439,0.));
#4749=DIRECTION('',(0.,0.,1.));
#4750=DIRECTION('',(-0.5,-0.866025403784439,0.));
#4751=DIRECTION('center_axis',(1.20185167898973E-16,1.,0.));
#4752=DIRECTION('ref_axis',(-1.,1.20185167898973E-16,0.));
#4753=DIRECTION('',(-1.,1.20185167898973E-16,0.));
#4754=DIRECTION('',(0.,0.,1.));
#4755=DIRECTION('',(-1.,1.20185167898973E-16,0.));
#4756=DIRECTION('center_axis',(0.866025403784439,0.5,0.));
#4757=DIRECTION('ref_axis',(-0.5,0.866025403784439,0.));
#4758=DIRECTION('',(-0.5,0.866025403784439,0.));
#4759=DIRECTION('',(0.,0.,1.));
#4760=DIRECTION('',(-0.5,0.866025403784439,0.));
#4761=DIRECTION('center_axis',(0.866025403784439,-0.5,0.));
#4762=DIRECTION('ref_axis',(0.5,0.866025403784439,0.));
#4763=DIRECTION('',(0.5,0.866025403784439,0.));
#4764=DIRECTION('',(0.5,0.866025403784439,0.));
#4765=DIRECTION('center_axis',(0.,0.,1.));
#4766=DIRECTION('ref_axis',(1.,0.,0.));
#4767=DIRECTION('center_axis',(0.,0.,1.));
#4768=DIRECTION('ref_axis',(1.,0.,0.));
#4769=DIRECTION('center_axis',(0.,0.,1.));
#4770=DIRECTION('ref_axis',(1.,0.,0.));
#4771=DIRECTION('center_axis',(0.,0.,1.));
#4772=DIRECTION('ref_axis',(1.,0.,0.));
#4773=DIRECTION('',(0.,0.,-1.));
#4774=DIRECTION('center_axis',(0.,0.,1.));
#4775=DIRECTION('ref_axis',(1.,0.,0.));
#4776=DIRECTION('center_axis',(0.,0.,1.));
#4777=DIRECTION('ref_axis',(1.,0.,0.));
#4778=DIRECTION('center_axis',(0.,0.,1.));
#4779=DIRECTION('ref_axis',(1.,0.,0.));
#4780=DIRECTION('axis',(0.,0.,1.));
#4781=DIRECTION('refdir',(1.,0.,0.));
#4782=DIRECTION('center_axis',(0.,0.,1.));
#4783=DIRECTION('ref_axis',(1.,0.,0.));
#4784=DIRECTION('center_axis',(0.,0.,1.));
#4785=DIRECTION('ref_axis',(1.,0.,0.));
#4786=DIRECTION('',(0.,0.,-1.));
#4787=DIRECTION('center_axis',(0.,0.,1.));
#4788=DIRECTION('ref_axis',(1.,0.,0.));
#4789=DIRECTION('center_axis',(0.,0.,1.));
#4790=DIRECTION('ref_axis',(1.,0.,0.));
#4791=DIRECTION('center_axis',(0.,0.,1.));
#4792=DIRECTION('ref_axis',(1.,0.,0.));
#4793=DIRECTION('',(0.,0.,1.));
#4794=DIRECTION('',(1.,0.,0.));
#4795=DIRECTION('',(0.,0.,1.));
#4796=DIRECTION('',(1.,0.,0.));
#4797=DIRECTION('',(0.,0.,1.));
#4798=DIRECTION('',(1.,0.,0.));
#4799=DIRECTION('',(1.,0.,0.));
#4800=DIRECTION('',(0.,1.,0.));
#4801=DIRECTION('',(1.,0.,0.));
#4802=DIRECTION('',(0.,1.,0.));
#4803=DIRECTION('',(1.,0.,0.));
#4804=DIRECTION('',(0.,1.,0.));
#4805=DIRECTION('',(1.,0.,0.));
#4806=DIRECTION('',(0.,1.,0.));
#4807=DIRECTION('',(1.,0.,0.));
#4808=DIRECTION('',(0.,1.,0.));
#4809=DIRECTION('',(1.,0.,0.));
#4810=DIRECTION('',(0.,1.,0.));
#4811=DIRECTION('',(0.,0.,1.));
#4812=DIRECTION('',(1.,0.,0.));
#4813=DIRECTION('',(0.,-1.22464679914735E-16,-1.));
#4814=DIRECTION('',(1.,0.,0.));
#4815=CARTESIAN_POINT('',(0.,0.,0.));
#4816=CARTESIAN_POINT('',(0.,0.,0.));
#4817=CARTESIAN_POINT('',(0.,0.,0.));
#4818=CARTESIAN_POINT('Origin',(-2.5,0.,-3.));
#4819=CARTESIAN_POINT('',(0.,-1.,-3.));
#4820=CARTESIAN_POINT('Origin',(0.,0.,-3.));
#4821=CARTESIAN_POINT('',(-5.,-1.,-3.));
#4822=CARTESIAN_POINT('',(-2.5,-1.,-3.));
#4823=CARTESIAN_POINT('Origin',(-5.,0.,-3.));
#4824=CARTESIAN_POINT('Origin',(-5.,0.,-3.));
#4825=CARTESIAN_POINT('Origin',(-2.5,0.,3.));
#4826=CARTESIAN_POINT('',(0.,-1.,3.));
#4827=CARTESIAN_POINT('Origin',(0.,0.,3.));
#4828=CARTESIAN_POINT('',(-5.,-1.,3.));
#4829=CARTESIAN_POINT('',(-2.5,-1.,3.));
#4830=CARTESIAN_POINT('Origin',(-5.,0.,3.));
#4831=CARTESIAN_POINT('Origin',(-5.,0.,3.));
#4832=CARTESIAN_POINT('Origin',(-6.,14.,-10.));
#4833=CARTESIAN_POINT('',(-12.,17.5,-10.));
#4834=CARTESIAN_POINT('Origin',(-12.,14.,-10.));
#4835=CARTESIAN_POINT('',(0.,17.5,-10.));
#4836=CARTESIAN_POINT('',(-6.,17.5,-10.));
#4837=CARTESIAN_POINT('Origin',(0.,14.,-10.));
#4838=CARTESIAN_POINT('Origin',(-6.,-14.,-10.));
#4839=CARTESIAN_POINT('',(-12.,-10.5,-10.));
#4840=CARTESIAN_POINT('Origin',(-12.,-14.,-10.));
#4841=CARTESIAN_POINT('',(0.,-10.5,-10.));
#4842=CARTESIAN_POINT('',(-6.,-10.5,-10.));
#4843=CARTESIAN_POINT('Origin',(0.,-14.,-10.));
#4844=CARTESIAN_POINT('Origin',(-6.,-14.,10.));
#4845=CARTESIAN_POINT('',(-12.,-10.5,10.));
#4846=CARTESIAN_POINT('Origin',(-12.,-14.,10.));
#4847=CARTESIAN_POINT('',(0.,-10.5,10.));
#4848=CARTESIAN_POINT('',(-6.,-10.5,10.));
#4849=CARTESIAN_POINT('Origin',(0.,-14.,10.));
#4850=CARTESIAN_POINT('Origin',(-6.,14.,10.));
#4851=CARTESIAN_POINT('',(-12.,17.5,10.));
#4852=CARTESIAN_POINT('Origin',(-12.,14.,10.));
#4853=CARTESIAN_POINT('',(0.,17.5,10.));
#4854=CARTESIAN_POINT('',(-6.,17.5,10.));
#4855=CARTESIAN_POINT('Origin',(0.,14.,10.));
#4856=CARTESIAN_POINT('Origin',(-6.,-6.,0.));
#4857=CARTESIAN_POINT('',(-12.,-3.,3.67394039744206E-16));
#4858=CARTESIAN_POINT('Origin',(-12.,-6.,0.));
#4859=CARTESIAN_POINT('',(0.,-3.,3.67394039744206E-16));
#4860=CARTESIAN_POINT('',(-6.,-3.,3.67394039744206E-16));
#4861=CARTESIAN_POINT('Origin',(0.,-6.,0.));
#4862=CARTESIAN_POINT('Origin',(-6.,6.,0.));
#4863=CARTESIAN_POINT('',(-12.,9.,3.67394039744206E-16));
#4864=CARTESIAN_POINT('Origin',(-12.,6.,0.));
#4865=CARTESIAN_POINT('',(0.,9.,3.67394039744206E-16));
#4866=CARTESIAN_POINT('',(-6.,9.,3.67394039744206E-16));
#4867=CARTESIAN_POINT('Origin',(0.,6.,0.));
#4868=CARTESIAN_POINT('Origin',(0.,20.,-15.));
#4869=CARTESIAN_POINT('',(0.,20.,-15.));
#4870=CARTESIAN_POINT('',(-12.,20.,-15.));
#4871=CARTESIAN_POINT('',(0.,20.,-15.));
#4872=CARTESIAN_POINT('',(-12.,20.,15.));
#4873=CARTESIAN_POINT('',(-12.,20.,-15.));
#4874=CARTESIAN_POINT('',(0.,20.,15.));
#4875=CARTESIAN_POINT('',(0.,20.,15.));
#4876=CARTESIAN_POINT('',(0.,20.,-15.));
#4877=CARTESIAN_POINT('Origin',(0.,-20.,-15.));
#4878=CARTESIAN_POINT('',(0.,-20.,-15.));
#4879=CARTESIAN_POINT('',(0.,-20.,-15.));
#4880=CARTESIAN_POINT('',(0.,-20.,15.));
#4881=CARTESIAN_POINT('',(0.,-20.,15.));
#4882=CARTESIAN_POINT('',(0.,-20.,-15.));
#4883=CARTESIAN_POINT('Origin',(-12.,-20.,-15.));
#4884=CARTESIAN_POINT('',(-12.,-20.,-15.));
#4885=CARTESIAN_POINT('',(-12.,-20.,-15.));
#4886=CARTESIAN_POINT('',(-12.,-20.,15.));
#4887=CARTESIAN_POINT('',(-12.,-20.,15.));
#4888=CARTESIAN_POINT('',(-12.,-20.,-15.));
#4889=CARTESIAN_POINT('Origin',(-12.,20.,-15.));
#4890=CARTESIAN_POINT('',(-12.,20.,-15.));
#4891=CARTESIAN_POINT('',(-12.,20.,15.));
#4892=CARTESIAN_POINT('Origin',(-6.,0.,15.));
#4893=CARTESIAN_POINT('Origin',(-6.,0.,-15.));
#4894=CARTESIAN_POINT('',(0.,0.,0.));
#4895=CARTESIAN_POINT('Origin',(6.,-6.,0.));
#4896=CARTESIAN_POINT('',(10.0890562790225,-3.88284304114924,0.00188038386388506));
#4897=CARTESIAN_POINT('',(10.3109437209775,-3.88619988433292,0.000572542807928916));
#4898=CARTESIAN_POINT('',(6.,-3.883,2.59257727379495E-16));
#4899=CARTESIAN_POINT('',(11.,-4.63708777074269,-1.61992569438875));
#4900=CARTESIAN_POINT('Ctrl Pts',(10.3109437209775,-3.88619988433292,0.000572542807928916));
#4901=CARTESIAN_POINT('Ctrl Pts',(10.3298470093174,-3.88540275069646,0.316007702174939));
#4902=CARTESIAN_POINT('Ctrl Pts',(10.3487502976573,-3.9515726183054,0.63113445646657));
#4903=CARTESIAN_POINT('Ctrl Pts',(10.3676535859971,-4.08639801625498,0.913504806799793));
#4904=CARTESIAN_POINT('Ctrl Pts',(10.4098100135973,-4.38707359317765,1.54322197643904));
#4905=CARTESIAN_POINT('Ctrl Pts',(10.4519664411975,-5.02920018705039,2.01002863635345));
#4906=CARTESIAN_POINT('Ctrl Pts',(10.4941228687977,-5.72080396656752,2.10193929805125));
#4907=CARTESIAN_POINT('Ctrl Pts',(10.5362792963979,-6.41240774608467,2.19384995974906));
#4908=CARTESIAN_POINT('Ctrl Pts',(10.5784357239981,-7.15348871124624,1.91086462323026));
#4909=CARTESIAN_POINT('Ctrl Pts',(10.6205921515983,-7.60833861494688,1.38152842182621));
#4910=CARTESIAN_POINT('Ctrl Pts',(10.6627485791985,-8.0631885186475,0.852192220422172));
#4911=CARTESIAN_POINT('Ctrl Pts',(10.7049050067987,-8.23180736088723,0.0765051541329273));
#4912=CARTESIAN_POINT('Ctrl Pts',(10.7470614343989,-8.03607510729347,-0.593437148822794));
#4913=CARTESIAN_POINT('Ctrl Pts',(10.789217861999,-7.8403428536997,-1.26337945177852));
#4914=CARTESIAN_POINT('Ctrl Pts',(10.8313742895992,-7.28025950427242,-1.82757699140071));
#4915=CARTESIAN_POINT('Ctrl Pts',(10.8735307171994,-6.61353338525505,-2.02952718354092));
#4916=CARTESIAN_POINT('Ctrl Pts',(10.9156871447996,-5.94680726623768,-2.23147737568112));
#4917=CARTESIAN_POINT('Ctrl Pts',(10.9578435723998,-5.1734383776302,-2.07118022033934));
#4918=CARTESIAN_POINT('Ctrl Pts',(11.,-4.63708777074269,-1.61992569438875));
#4919=CARTESIAN_POINT('',(11.,-4.63477372010686,1.62290954611129));
#4920=CARTESIAN_POINT('Origin',(11.,-6.,0.));
#4921=CARTESIAN_POINT('',(10.8890562790225,-3.88056244769026,-0.00125294615386077));
#4922=CARTESIAN_POINT('Ctrl Pts',(11.,-4.63477280471474,1.62291072646332));
#4923=CARTESIAN_POINT('Ctrl Pts',(10.9630187596742,-4.1668044376417,1.22807503995787));
#4924=CARTESIAN_POINT('Ctrl Pts',(10.9260375193483,-3.88442940297563,0.611672206073652));
#4925=CARTESIAN_POINT('Ctrl Pts',(10.8890562790225,-3.88056244769026,-0.00125294615386077));
#4926=CARTESIAN_POINT('',(12.,-3.883,-2.59257727379495E-16));
#4927=CARTESIAN_POINT('',(6.,-3.883,2.59257727379495E-16));
#4928=CARTESIAN_POINT('Origin',(12.,-6.,0.));
#4929=CARTESIAN_POINT('Ctrl Pts',(10.8890562790225,-3.88056244769026,-0.00125294615386077));
#4930=CARTESIAN_POINT('Ctrl Pts',(10.8848236262981,-3.8801198589972,-0.0714047120918237));
#4931=CARTESIAN_POINT('Ctrl Pts',(10.8805909735737,-3.88332565081622,-0.141510921340689));
#4932=CARTESIAN_POINT('Ctrl Pts',(10.8763583208493,-3.89031913181604,-0.211234160340694));
#4933=CARTESIAN_POINT('Ctrl Pts',(10.8342018932491,-3.95997289144109,-0.905664549114537));
#4934=CARTESIAN_POINT('Ctrl Pts',(10.7920454656489,-4.40535733277697,-1.56210510667178));
#4935=CARTESIAN_POINT('Ctrl Pts',(10.7498890380487,-5.02491685437878,-1.88289988652445));
#4936=CARTESIAN_POINT('Ctrl Pts',(10.7077326104485,-5.6444763759806,-2.20369466637711));
#4937=CARTESIAN_POINT('Ctrl Pts',(10.6655761828483,-6.43821097784834,-2.1888436685252));
#4938=CARTESIAN_POINT('Ctrl Pts',(10.6234197552481,-7.04536578251427,-1.84487773284302));
#4939=CARTESIAN_POINT('Ctrl Pts',(10.5812633276479,-7.65252058718018,-1.50091179716084));
#4940=CARTESIAN_POINT('Ctrl Pts',(10.5391069000478,-8.07309559464429,-0.827830923648425));
#4941=CARTESIAN_POINT('Ctrl Pts',(10.4969504724476,-8.11630674809371,-0.131366079627778));
#4942=CARTESIAN_POINT('Ctrl Pts',(10.4547940448474,-8.15951790154314,0.565098764392898));
#4943=CARTESIAN_POINT('Ctrl Pts',(10.4126376172472,-7.82536520097785,1.2849475789218));
#4944=CARTESIAN_POINT('Ctrl Pts',(10.370481189647,-7.26547901823063,1.70138266663689));
#4945=CARTESIAN_POINT('Ctrl Pts',(10.3283247620468,-6.70559283548343,2.11781775435196));
#4946=CARTESIAN_POINT('Ctrl Pts',(10.2861683344466,-5.91997317055431,2.23083911525323));
#4947=CARTESIAN_POINT('Ctrl Pts',(10.2440119068464,-5.26538953182608,1.98909784789284));
#4948=CARTESIAN_POINT('Ctrl Pts',(10.2018554792462,-4.61080589309784,1.74735658053246));
#4949=CARTESIAN_POINT('Ctrl Pts',(10.159699051646,-4.08725828057048,1.15085268491044));
#4950=CARTESIAN_POINT('Ctrl Pts',(10.1175426240458,-3.93244343062105,0.470451404639381));
#4951=CARTESIAN_POINT('Ctrl Pts',(10.1080471757047,-3.89757243955716,0.317195648024649));
#4952=CARTESIAN_POINT('Ctrl Pts',(10.0985517273636,-3.88140891929161,0.159683399899897));
#4953=CARTESIAN_POINT('Ctrl Pts',(10.0890562790225,-3.88284304114924,0.00188038386388506));
#4954=CARTESIAN_POINT('Origin',(6.,-6.,0.));
#4955=CARTESIAN_POINT('',(9.28905627902251,-3.88625832207874,-0.000568483867972452));
#4956=CARTESIAN_POINT('',(9.5109437209775,-3.88285291798587,-0.00188412158878793));
#4957=CARTESIAN_POINT('',(6.,-3.883,2.59257727379495E-16));
#4958=CARTESIAN_POINT('Ctrl Pts',(9.5109437209775,-3.88285291798587,-0.00188412158878793));
#4959=CARTESIAN_POINT('Ctrl Pts',(9.5435751103829,-3.88777973151044,0.540420553202403));
#4960=CARTESIAN_POINT('Ctrl Pts',(9.5762064997883,-4.10049090304194,1.08616069834087));
#4961=CARTESIAN_POINT('Ctrl Pts',(9.6088378891937,-4.47605139447185,1.4743533520236));
#4962=CARTESIAN_POINT('Ctrl Pts',(9.65099431679389,-4.9612372524739,1.97585867552033));
#4963=CARTESIAN_POINT('Ctrl Pts',(9.69315074439408,-5.71821870890957,2.21441715497353));
#4964=CARTESIAN_POINT('Ctrl Pts',(9.73530717199427,-6.40327135435487,2.08170804052273));
#4965=CARTESIAN_POINT('Ctrl Pts',(9.77746359959446,-7.08832399980019,1.94899892607192));
#4966=CARTESIAN_POINT('Ctrl Pts',(9.81962002719465,-7.70144783425515,1.44502221771709));
#4967=CARTESIAN_POINT('Ctrl Pts',(9.86177645479484,-7.96426282646742,0.798615346598204));
#4968=CARTESIAN_POINT('Ctrl Pts',(9.90393288239503,-8.22707781867969,0.152208475479324));
#4969=CARTESIAN_POINT('Ctrl Pts',(9.94608930999523,-8.1395839686493,-0.636628558403595));
#4970=CARTESIAN_POINT('Ctrl Pts',(9.98824573759542,-7.74147846610521,-1.20971721337014));
#4971=CARTESIAN_POINT('Ctrl Pts',(10.0304021651956,-7.34337296356112,-1.78280586833669));
#4972=CARTESIAN_POINT('Ctrl Pts',(10.0725585927958,-6.63465580850333,-2.14014614438684));
#4973=CARTESIAN_POINT('Ctrl Pts',(10.114715020396,-5.9371863419647,-2.11947983260037));
#4974=CARTESIAN_POINT('Ctrl Pts',(10.1568714479962,-5.23971687542607,-2.0988135208139));
#4975=CARTESIAN_POINT('Ctrl Pts',(10.1990278755964,-4.5534950974066,-1.70014062119081));
#4976=CARTESIAN_POINT('Ctrl Pts',(10.2411843031966,-4.18999648838316,-1.1044903316972));
#4977=CARTESIAN_POINT('Ctrl Pts',(10.2644374424569,-3.98949364082893,-0.775934523709865));
#4978=CARTESIAN_POINT('Ctrl Pts',(10.2876905817172,-3.88718044703313,-0.387447655396757));
#4979=CARTESIAN_POINT('Ctrl Pts',(10.3109437209775,-3.88619988433292,0.000572542807928916));
#4980=CARTESIAN_POINT('Ctrl Pts',(10.0890562790225,-3.88284304114924,0.00188038386388506));
#4981=CARTESIAN_POINT('Ctrl Pts',(10.0563952997634,-3.88777591241182,-0.540906101683727));
#4982=CARTESIAN_POINT('Ctrl Pts',(10.0237343205043,-4.10090936331863,-1.08713270990473));
#4983=CARTESIAN_POINT('Ctrl Pts',(9.99107334124527,-4.4770789027728,-1.47541427191919));
#4984=CARTESIAN_POINT('Ctrl Pts',(9.94891691364508,-4.96261131224547,-1.97658000328661));
#4985=CARTESIAN_POINT('Ctrl Pts',(9.90676048604489,-5.71975821856232,-2.21461280110137));
#4986=CARTESIAN_POINT('Ctrl Pts',(9.8646040584447,-6.40472126940695,-2.08142682840507));
#4987=CARTESIAN_POINT('Ctrl Pts',(9.82244763084451,-7.0896843202516,-1.94824085570876));
#4988=CARTESIAN_POINT('Ctrl Pts',(9.78029120324431,-7.70246351562404,-1.44383611250138));
#4989=CARTESIAN_POINT('Ctrl Pts',(9.73813477564412,-7.9648231489573,-0.797245612832521));
#4990=CARTESIAN_POINT('Ctrl Pts',(9.69597834804393,-8.22718278229054,-0.150655113163675));
#4991=CARTESIAN_POINT('Ctrl Pts',(9.65382192044375,-8.13912285358463,0.638121142966619));
#4992=CARTESIAN_POINT('Ctrl Pts',(9.61166549284356,-7.74062604192175,1.21093142563168));
#4993=CARTESIAN_POINT('Ctrl Pts',(9.56950906524337,-7.34212923025887,1.78374170829674));
#4994=CARTESIAN_POINT('Ctrl Pts',(9.52735263764317,-6.63319553563902,2.14058601749655));
#4995=CARTESIAN_POINT('Ctrl Pts',(9.48519621004298,-5.93572544911276,2.11943448582987));
#4996=CARTESIAN_POINT('Ctrl Pts',(9.44303978244279,-5.23825536258647,2.09828295416318));
#4997=CARTESIAN_POINT('Ctrl Pts',(9.4008833548426,-4.55224888415376,1.69913558162997));
#4998=CARTESIAN_POINT('Ctrl Pts',(9.35872692724241,-4.18919459490055,1.1032301330012));
#4999=CARTESIAN_POINT('Ctrl Pts',(9.33550337783578,-3.98919166050286,0.774951850999683));
#5000=CARTESIAN_POINT('Ctrl Pts',(9.31227982842914,-3.88719814718334,0.386961494651881));
#5001=CARTESIAN_POINT('Ctrl Pts',(9.28905627902251,-3.88625832207874,-0.000568483867972452));
#5002=CARTESIAN_POINT('Origin',(6.,-6.,0.));
#5003=CARTESIAN_POINT('',(8.4890562790225,-3.88081569696024,-0.00138638344793468));
#5004=CARTESIAN_POINT('',(8.7109437209775,-3.88042895428249,0.00117038079968268));
#5005=CARTESIAN_POINT('',(6.,-3.883,2.59257727379495E-16));
#5006=CARTESIAN_POINT('Ctrl Pts',(8.7109437209775,-3.88042895428249,0.00117038079968268));
#5007=CARTESIAN_POINT('Ctrl Pts',(8.71514678384823,-3.87996428152845,0.0708143797887767));
#5008=CARTESIAN_POINT('Ctrl Pts',(8.71934984671896,-3.88310204798081,0.140416007857776));
#5009=CARTESIAN_POINT('Ctrl Pts',(8.72355290958969,-3.88998055273578,0.209645965979184));
#5010=CARTESIAN_POINT('Ctrl Pts',(8.76570933718988,-3.95897147593134,0.904017619954446));
#5011=CARTESIAN_POINT('Ctrl Pts',(8.80786576479007,-4.40427880810987,1.56099946242998));
#5012=CARTESIAN_POINT('Ctrl Pts',(8.85002219239026,-5.02370573481769,1.88228135692562));
#5013=CARTESIAN_POINT('Ctrl Pts',(8.89217861999045,-5.64313266152551,2.20356325142126));
#5014=CARTESIAN_POINT('Ctrl Pts',(8.93433504759064,-6.43667918276262,2.189145197937));
#5015=CARTESIAN_POINT('Ctrl Pts',(8.97649147519083,-7.04402622875504,1.84557386816763));
#5016=CARTESIAN_POINT('Ctrl Pts',(9.01864790279102,-7.65137327474745,1.50200253839825));
#5017=CARTESIAN_POINT('Ctrl Pts',(9.06080433039121,-8.07252084549518,0.829277932343754));
#5018=CARTESIAN_POINT('Ctrl Pts',(9.1029607579914,-8.11624237804386,0.132858395408587));
#5019=CARTESIAN_POINT('Ctrl Pts',(9.14511718559159,-8.15996391059253,-0.563561141526579));
#5020=CARTESIAN_POINT('Ctrl Pts',(9.18727361319179,-7.82625940494216,-1.28367560934241));
#5021=CARTESIAN_POINT('Ctrl Pts',(9.22943004079198,-7.26665060216368,-1.70050881300008));
#5022=CARTESIAN_POINT('Ctrl Pts',(9.27158646839217,-6.7070417993852,-2.11734201665774));
#5023=CARTESIAN_POINT('Ctrl Pts',(9.31374289599236,-5.9215286994786,-2.23089395615724));
#5024=CARTESIAN_POINT('Ctrl Pts',(9.35589932359255,-5.26678371915212,-1.9896049943898));
#5025=CARTESIAN_POINT('Ctrl Pts',(9.39805575119274,-4.61203873882566,-1.74831603262238));
#5026=CARTESIAN_POINT('Ctrl Pts',(9.44021217879293,-4.0880618780793,-1.15218616958803));
#5027=CARTESIAN_POINT('Ctrl Pts',(9.48236860639312,-3.93276857749032,-0.471895154300735));
#5028=CARTESIAN_POINT('Ctrl Pts',(9.49189364458792,-3.89768081736193,-0.318186733709686));
#5029=CARTESIAN_POINT('Ctrl Pts',(9.50141868278271,-3.88141479083728,-0.16018178634426));
#5030=CARTESIAN_POINT('Ctrl Pts',(9.5109437209775,-3.88285291798587,-0.00188412158878793));
#5031=CARTESIAN_POINT('Ctrl Pts',(9.28905627902251,-3.88625832207874,-0.000568483867972452));
#5032=CARTESIAN_POINT('Ctrl Pts',(9.27012340082895,-3.88549213453708,-0.316500288744127));
#5033=CARTESIAN_POINT('Ctrl Pts',(9.25119052263539,-3.95188866409716,-0.632126115418351));
#5034=CARTESIAN_POINT('Ctrl Pts',(9.23225764444183,-4.08709739014463,-0.91484264263593));
#5035=CARTESIAN_POINT('Ctrl Pts',(9.19010121684164,-4.38815657471562,-1.54434644491999));
#5036=CARTESIAN_POINT('Ctrl Pts',(9.14794478924145,-5.03037704393129,-2.01069052476379));
#5037=CARTESIAN_POINT('Ctrl Pts',(9.10578836164126,-5.72215108182613,-2.10212591529422));
#5038=CARTESIAN_POINT('Ctrl Pts',(9.06363193404107,-6.41392511972096,-2.19356130582466));
#5039=CARTESIAN_POINT('Ctrl Pts',(9.02147550644088,-7.15525272629495,-1.91008800704174));
#5040=CARTESIAN_POINT('Ctrl Pts',(8.97931907884069,-7.6095256731943,-1.38042036796998));
#5041=CARTESIAN_POINT('Ctrl Pts',(8.9371626512405,-8.06379862009367,-0.850752728898211));
#5042=CARTESIAN_POINT('Ctrl Pts',(8.89500622364031,-8.23101690731839,-0.0748907495375924));
#5043=CARTESIAN_POINT('Ctrl Pts',(8.85284979604012,-8.03525311381774,0.594876562001453));
#5044=CARTESIAN_POINT('Ctrl Pts',(8.81069336843993,-7.8394893203171,1.26464387354049));
#5045=CARTESIAN_POINT('Ctrl Pts',(8.76853694083974,-7.28074344609107,1.82831651725797));
#5046=CARTESIAN_POINT('Ctrl Pts',(8.72638051323955,-6.6127204856351,2.02995245057092));
#5047=CARTESIAN_POINT('Ctrl Pts',(8.68422408563935,-5.94469752517913,2.23158838388388));
#5048=CARTESIAN_POINT('Ctrl Pts',(8.64206765803916,-5.1673974784932,2.07118760679231));
#5049=CARTESIAN_POINT('Ctrl Pts',(8.59991123043897,-4.63376233782377,1.62158193871465));
#5050=CARTESIAN_POINT('Ctrl Pts',(8.56295957996681,-4.16601162173637,1.22748612835167));
#5051=CARTESIAN_POINT('Ctrl Pts',(8.52600792949465,-3.88547263914832,0.611189469031259));
#5052=CARTESIAN_POINT('Ctrl Pts',(8.4890562790225,-3.88081569696024,-0.00138638344793468));
#5053=CARTESIAN_POINT('Origin',(6.,-6.,0.));
#5054=CARTESIAN_POINT('',(7.68905627902251,-3.88235469492868,0.00183633483374523));
#5055=CARTESIAN_POINT('',(7.9109437209775,-3.88609278259416,0.000819409314603885));
#5056=CARTESIAN_POINT('',(6.,-3.883,2.59257727379495E-16));
#5057=CARTESIAN_POINT('Ctrl Pts',(7.9109437209775,-3.88609278259416,0.000819409314603885));
#5058=CARTESIAN_POINT('Ctrl Pts',(7.92887488491375,-3.88504204554916,0.299977116189444));
#5059=CARTESIAN_POINT('Ctrl Pts',(7.94680604885,-3.94433953053336,0.598737191648719));
#5060=CARTESIAN_POINT('Ctrl Pts',(7.96473721278625,-4.06603975290357,0.869443107203424));
#5061=CARTESIAN_POINT('Ctrl Pts',(8.00689364038644,-4.35215874838639,1.505876657786));
#5062=CARTESIAN_POINT('Ctrl Pts',(8.04905006798663,-4.98319449029903,1.98724730626784));
#5063=CARTESIAN_POINT('Ctrl Pts',(8.09120649558682,-5.67261796286648,2.09498318776012));
#5064=CARTESIAN_POINT('Ctrl Pts',(8.13336292318701,-6.36204143543391,2.2027190692524));
#5065=CARTESIAN_POINT('Ctrl Pts',(8.1755193507872,-7.10985263865614,1.93682018375513));
#5066=CARTESIAN_POINT('Ctrl Pts',(8.21767577838739,-7.57649931373914,1.41802097027599));
#5067=CARTESIAN_POINT('Ctrl Pts',(8.25983220598758,-8.04314598882215,0.899221756796831));
#5068=CARTESIAN_POINT('Ctrl Pts',(8.30198863358777,-8.22862813576591,0.127522215335779));
#5069=CARTESIAN_POINT('Ctrl Pts',(8.34414506118797,-8.04872546454541,-0.546678624303283));
#5070=CARTESIAN_POINT('Ctrl Pts',(8.38630148878816,-7.86882279332492,-1.22087946394234));
#5071=CARTESIAN_POINT('Ctrl Pts',(8.42845791638835,-7.32353530394018,-1.7975816017594));
#5072=CARTESIAN_POINT('Ctrl Pts',(8.47061434398854,-6.66045702367441,-2.01492681722953));
#5073=CARTESIAN_POINT('Ctrl Pts',(8.51277077158873,-5.99737874340865,-2.23227203269965));
#5074=CARTESIAN_POINT('Ctrl Pts',(8.55492719918892,-5.21650967226187,-2.09026032582285));
#5075=CARTESIAN_POINT('Ctrl Pts',(8.59708362678911,-4.67241239379476,-1.65337373964697));
#5076=CARTESIAN_POINT('Ctrl Pts',(8.63503699151858,-4.18256247923803,-1.2600454408689));
#5077=CARTESIAN_POINT('Ctrl Pts',(8.67299035624804,-3.88462491685935,-0.627710075226815));
#5078=CARTESIAN_POINT('Ctrl Pts',(8.7109437209775,-3.88042895428249,0.00117038079968268));
#5079=CARTESIAN_POINT('Ctrl Pts',(8.4890562790225,-3.88081569696024,-0.00138638344793468));
#5080=CARTESIAN_POINT('Ctrl Pts',(8.48385150189447,-3.88015974936717,-0.0876699660601046));
#5081=CARTESIAN_POINT('Ctrl Pts',(8.47864672476643,-3.88497723749026,-0.173879728727243));
#5082=CARTESIAN_POINT('Ctrl Pts',(8.4734419476384,-3.89551595094417,-0.259384332255975));
#5083=CARTESIAN_POINT('Ctrl Pts',(8.4312855200382,-3.98087493938691,-0.951934376085218));
#5084=CARTESIAN_POINT('Ctrl Pts',(8.38912909243802,-4.44156315092533,-1.59822390467993));
#5085=CARTESIAN_POINT('Ctrl Pts',(8.34697266483782,-5.06839981536676,-1.90479774186325));
#5086=CARTESIAN_POINT('Ctrl Pts',(8.30481623723763,-5.69523647980819,-2.21137157904657));
#5087=CARTESIAN_POINT('Ctrl Pts',(8.26265980963744,-6.48822159715263,-2.17822972481849));
#5088=CARTESIAN_POINT('Ctrl Pts',(8.22050338203725,-7.08729117964857,-1.82042061921142));
#5089=CARTESIAN_POINT('Ctrl Pts',(8.17834695443706,-7.68636076214451,-1.46261151360435));
#5090=CARTESIAN_POINT('Ctrl Pts',(8.13619052683687,-8.09151480979196,-0.780135156618282));
#5091=CARTESIAN_POINT('Ctrl Pts',(8.09403409923668,-8.11878847871396,-0.0828777667085811));
#5092=CARTESIAN_POINT('Ctrl Pts',(8.05187767163649,-8.14606214763596,0.61437962320112));
#5093=CARTESIAN_POINT('Ctrl Pts',(8.00972124403629,-7.79545543783251,1.32641804603445));
#5094=CARTESIAN_POINT('Ctrl Pts',(7.9675648164361,-7.22616534830724,1.72992828747435));
#5095=CARTESIAN_POINT('Ctrl Pts',(7.92540838883591,-6.65687525878197,2.13343852891425));
#5096=CARTESIAN_POINT('Ctrl Pts',(7.88325196123572,-5.86890178953488,2.22842058896072));
#5097=CARTESIAN_POINT('Ctrl Pts',(7.84109553363553,-5.2200333333253,1.97174677379236));
#5098=CARTESIAN_POINT('Ctrl Pts',(7.79893910603534,-4.57116487711572,1.71507295862401));
#5099=CARTESIAN_POINT('Ctrl Pts',(7.75678267843515,-4.06140143394366,1.10674326824082));
#5100=CARTESIAN_POINT('Ctrl Pts',(7.71462625083496,-3.92220694306612,0.422976776968435));
#5101=CARTESIAN_POINT('Ctrl Pts',(7.70610292689748,-3.89406414720794,0.284730639084455));
#5102=CARTESIAN_POINT('Ctrl Pts',(7.69757960295999,-3.88106949506508,0.143400790343917));
#5103=CARTESIAN_POINT('Ctrl Pts',(7.68905627902251,-3.88235469492868,0.00183633483374523));
#5104=CARTESIAN_POINT('Origin',(6.,-6.,0.));
#5105=CARTESIAN_POINT('',(6.8890562790225,-3.88636003231944,-0.00031417126607286));
#5106=CARTESIAN_POINT('',(7.1109437209775,-3.88333340233497,-0.00189050360831077));
#5107=CARTESIAN_POINT('',(6.,-3.883,2.59257727379495E-16));
#5108=CARTESIAN_POINT('Ctrl Pts',(7.1109437209775,-3.88333340233497,-0.00189050360831077));
#5109=CARTESIAN_POINT('Ctrl Pts',(7.14260298597927,-3.88803082624995,0.524564043326856));
#5110=CARTESIAN_POINT('Ctrl Pts',(7.17426225098104,-4.087035328391,1.05418914371193));
#5111=CARTESIAN_POINT('Ctrl Pts',(7.20592151598281,-4.4426850828802,1.43906351629628));
#5112=CARTESIAN_POINT('Ctrl Pts',(7.248077943583,-4.91625650424173,1.95154947015887));
#5113=CARTESIAN_POINT('Ctrl Pts',(7.29023437118319,-5.66757096416104,2.20738221321448));
#5114=CARTESIAN_POINT('Ctrl Pts',(7.33239079878338,-6.35548551341645,2.09039795368626));
#5115=CARTESIAN_POINT('Ctrl Pts',(7.37454722638357,-7.04340006267187,1.97341369415804));
#5116=CARTESIAN_POINT('Ctrl Pts',(7.41670365398376,-7.66791470126341,1.483612432046));
#5117=CARTESIAN_POINT('Ctrl Pts',(7.45886008158396,-7.9454613933261,0.843394049180934));
#5118=CARTESIAN_POINT('Ctrl Pts',(7.50101650918415,-8.22300808538879,0.203175666315868));
#5119=CARTESIAN_POINT('Ctrl Pts',(7.54317293678433,-8.15358683092263,-0.587459837302209));
#5120=CARTESIAN_POINT('Ctrl Pts',(7.58532936438453,-7.76871914701981,-1.16951534144242));
#5121=CARTESIAN_POINT('Ctrl Pts',(7.62748579198471,-7.38385146311698,-1.75157084558263));
#5122=CARTESIAN_POINT('Ctrl Pts',(7.66964221958491,-6.6835373497775,-2.12504635024497));
#5123=CARTESIAN_POINT('Ctrl Pts',(7.7117986471851,-5.98576246358723,-2.12036101821588));
#5124=CARTESIAN_POINT('Ctrl Pts',(7.75395507478529,-5.28798757739695,-2.1156756861868));
#5125=CARTESIAN_POINT('Ctrl Pts',(7.79611150238548,-4.59275191835588,-1.7328295174663));
#5126=CARTESIAN_POINT('Ctrl Pts',(7.83826792998567,-4.21573521336184,-1.14565820676439));
#5127=CARTESIAN_POINT('Ctrl Pts',(7.86249319364961,-3.9990819150603,-0.80823920265523));
#5128=CARTESIAN_POINT('Ctrl Pts',(7.88671845731356,-3.88751234364703,-0.403347010216734));
#5129=CARTESIAN_POINT('Ctrl Pts',(7.9109437209775,-3.88609278259416,0.000819409314603885));
#5130=CARTESIAN_POINT('Ctrl Pts',(7.68905627902251,-3.88235469492868,0.00183633483374523));
#5131=CARTESIAN_POINT('Ctrl Pts',(7.6554231753598,-3.88742610375424,-0.556778126150017));
#5132=CARTESIAN_POINT('Ctrl Pts',(7.62179007169709,-4.11484877990915,-1.11904564407922));
#5133=CARTESIAN_POINT('Ctrl Pts',(7.58815696803438,-4.51127209883019,-1.50990813544534));
#5134=CARTESIAN_POINT('Ctrl Pts',(7.54600054043419,-5.00815728405479,-1.99982326442516));
#5135=CARTESIAN_POINT('Ctrl Pts',(7.503844112834,-5.770553193087,-2.22045023022322));
#5136=CARTESIAN_POINT('Ctrl Pts',(7.46168768523381,-6.45228521760907,-2.07161082810745));
#5137=CARTESIAN_POINT('Ctrl Pts',(7.41953125763362,-7.13401724213114,-1.92277142599167));
#5138=CARTESIAN_POINT('Ctrl Pts',(7.37737483003343,-7.73508538214306,-1.40446565596207));
#5139=CARTESIAN_POINT('Ctrl Pts',(7.33521840243324,-7.98256775348064,-0.752036198654528));
#5140=CARTESIAN_POINT('Ctrl Pts',(7.29306197483304,-8.23005012481823,-0.0996067413469874));
#5141=CARTESIAN_POINT('Ctrl Pts',(7.25090554723286,-8.12394672748148,0.686946403238489));
#5142=CARTESIAN_POINT('Ctrl Pts',(7.20874911963266,-7.71243502620873,1.25047975682414));
#5143=CARTESIAN_POINT('Ctrl Pts',(7.16659269203247,-7.30092332493598,1.81401311040979));
#5144=CARTESIAN_POINT('Ctrl Pts',(7.12443626443228,-6.58400331972723,2.15452667299561));
#5145=CARTESIAN_POINT('Ctrl Pts',(7.08227983683209,-5.88720076311748,2.11740635527826));
#5146=CARTESIAN_POINT('Ctrl Pts',(7.0401234092319,-5.19039820650772,2.08028603756091));
#5147=CARTESIAN_POINT('Ctrl Pts',(6.99796698163171,-4.51371309849697,1.66553183954039));
#5148=CARTESIAN_POINT('Ctrl Pts',(6.95581055403152,-4.16440207499811,1.06146766269465));
#5149=CARTESIAN_POINT('Ctrl Pts',(6.93355912902851,-3.98002525550516,0.742624499427559));
#5150=CARTESIAN_POINT('Ctrl Pts',(6.91130770402551,-3.88685631420567,0.37103873280126));
#5151=CARTESIAN_POINT('Ctrl Pts',(6.8890562790225,-3.88636003231944,-0.00031417126607286));
#5152=CARTESIAN_POINT('Origin',(6.,-6.,0.));
#5153=CARTESIAN_POINT('',(6.0890562790225,-3.88123446329707,-0.00156260716336218));
#5154=CARTESIAN_POINT('',(6.3109437209775,-3.88010896117177,0.000931372864572485));
#5155=CARTESIAN_POINT('',(6.,-3.883,2.59257727379495E-16));
#5156=CARTESIAN_POINT('Ctrl Pts',(6.3109437209775,-3.88010896117177,0.000931372864572485));
#5157=CARTESIAN_POINT('Ctrl Pts',(6.3141746594446,-3.87981270635624,0.0544460888779948));
#5158=CARTESIAN_POINT('Ctrl Pts',(6.3174055979117,-3.88166513255228,0.107939967166579));
#5159=CARTESIAN_POINT('Ctrl Pts',(6.3206365363788,-3.88573247061989,0.161264903944568));
#5160=CARTESIAN_POINT('Ctrl Pts',(6.36279296397899,-3.93880201821999,0.857034526132367));
#5161=CARTESIAN_POINT('Ctrl Pts',(6.40494939157918,-4.36894564474271,1.52404297487717));
#5162=CARTESIAN_POINT('Ctrl Pts',(6.44710581917937,-4.98085170215647,1.85942741241423));
#5163=CARTESIAN_POINT('Ctrl Pts',(6.48926224677956,-5.59275775957023,2.19481184995129));
#5164=CARTESIAN_POINT('Ctrl Pts',(6.53141867437975,-6.38642624787501,2.19857227628061));
#5165=CARTESIAN_POINT('Ctrl Pts',(6.57357510197994,-7.00148288535931,1.86900122668953));
#5166=CARTESIAN_POINT('Ctrl Pts',(6.61573152958014,-7.6165395228436,1.53943017709846));
#5167=CARTESIAN_POINT('Ctrl Pts',(6.65788795718033,-8.05298430950739,0.876527651586999));
#5168=CARTESIAN_POINT('Ctrl Pts',(6.70004438478052,-8.11264448327204,0.181292146374433));
#5169=CARTESIAN_POINT('Ctrl Pts',(6.74220081238071,-8.17230465703668,-0.513943358838142));
#5170=CARTESIAN_POINT('Ctrl Pts',(6.7843572399809,-7.85518021790216,-1.24151184375183));
#5171=CARTESIAN_POINT('Ctrl Pts',(6.82651366758109,-7.30526515536498,-1.67105249146255));
#5172=CARTESIAN_POINT('Ctrl Pts',(6.86867009518128,-6.7553500928278,-2.10059313917327));
#5173=CARTESIAN_POINT('Ctrl Pts',(6.91082652278147,-5.97264440688797,-2.23210594968102));
#5174=CARTESIAN_POINT('Ctrl Pts',(6.95298295038166,-5.31254459307855,-2.00587602272101));
#5175=CARTESIAN_POINT('Ctrl Pts',(6.99513937798185,-4.65244477926912,-1.779646095761));
#5176=CARTESIAN_POINT('Ctrl Pts',(7.03729580558204,-4.11495083759011,-1.19567343133322));
#5177=CARTESIAN_POINT('Ctrl Pts',(7.07945223318223,-3.94411805815251,-0.519117516784533));
#5178=CARTESIAN_POINT('Ctrl Pts',(7.08994939578066,-3.90157983646295,-0.350651689715541));
#5179=CARTESIAN_POINT('Ctrl Pts',(7.10044655837907,-3.88177589230982,-0.176445376551414));
#5180=CARTESIAN_POINT('Ctrl Pts',(7.1109437209775,-3.88333340233497,-0.00189050360831077));
#5181=CARTESIAN_POINT('Ctrl Pts',(6.8890562790225,-3.88636003231944,-0.00031417126607286));
#5182=CARTESIAN_POINT('Ctrl Pts',(6.86915127642532,-3.8859160835731,-0.33250775073049));
#5183=CARTESIAN_POINT('Ctrl Pts',(6.84924627382813,-3.95963055094797,-0.664514989167724));
#5184=CARTESIAN_POINT('Ctrl Pts',(6.82934127123095,-4.10855197683347,-0.958414167713982));
#5185=CARTESIAN_POINT('Ctrl Pts',(6.78718484363076,-4.42394984115464,-1.58085766560597));
#5186=CARTESIAN_POINT('Ctrl Pts',(6.74502841603057,-5.07668250878394,-2.03237050571901));
#5187=CARTESIAN_POINT('Ctrl Pts',(6.70287198843038,-5.77036922413792,-2.10793810345388));
#5188=CARTESIAN_POINT('Ctrl Pts',(6.66071556083019,-6.46405593949191,-2.18350570118874));
#5189=CARTESIAN_POINT('Ctrl Pts',(6.61855913322999,-7.19869670257056,-1.88312805654543));
#5190=CARTESIAN_POINT('Ctrl Pts',(6.5764027056298,-7.64071944743897,-1.34319508486732));
#5191=CARTESIAN_POINT('Ctrl Pts',(6.53424627802961,-8.08274219230738,-0.803262113189214));
#5192=CARTESIAN_POINT('Ctrl Pts',(6.49208985042942,-8.23214691896553,-0.0237738144762983));
#5193=CARTESIAN_POINT('Ctrl Pts',(6.44993342282923,-8.0210946973726,0.641334207311783));
#5194=CARTESIAN_POINT('Ctrl Pts',(6.40777699522904,-7.81004247577966,1.30644222909986));
#5195=CARTESIAN_POINT('Ctrl Pts',(6.36562056762885,-7.23853330593564,1.85716997396313));
#5196=CARTESIAN_POINT('Ctrl Pts',(6.32346414002865,-6.56606748249676,2.04345319165272));
#5197=CARTESIAN_POINT('Ctrl Pts',(6.28130771242846,-5.89360165905787,2.22973640934232));
#5198=CARTESIAN_POINT('Ctrl Pts',(6.23915128482827,-5.12017918202413,2.05157509985824));
#5199=CARTESIAN_POINT('Ctrl Pts',(6.19699485722808,-4.59698139943735,1.58986544955578));
#5200=CARTESIAN_POINT('Ctrl Pts',(6.16101533115955,-4.15044431531567,1.19580704980958));
#5201=CARTESIAN_POINT('Ctrl Pts',(6.12503580509103,-3.8861764962572,0.595205695519721));
#5202=CARTESIAN_POINT('Ctrl Pts',(6.0890562790225,-3.88123446329707,-0.00156260716336218));
#5203=CARTESIAN_POINT('Origin',(6.,-6.,0.));
#5204=CARTESIAN_POINT('',(5.2890562790225,-3.88187782281943,0.00175000188907953));
#5205=CARTESIAN_POINT('',(5.51094372097749,-3.88587578853395,0.0010475127251217));
#5206=CARTESIAN_POINT('',(6.,-3.883,2.59257727379495E-16));
#5207=CARTESIAN_POINT('Ctrl Pts',(5.51094372097749,-3.88587578853395,0.0010475127251217));
#5208=CARTESIAN_POINT('Ctrl Pts',(5.52790276051011,-3.88459758142574,0.283913878504502));
#5209=CARTESIAN_POINT('Ctrl Pts',(5.54486180004273,-3.93742581719468,0.566322436662692));
#5210=CARTESIAN_POINT('Ctrl Pts',(5.56182083957536,-4.0466340760357,0.824921282384071));
#5211=CARTESIAN_POINT('Ctrl Pts',(5.60397726717555,-4.31810169354546,1.46774091236234));
#5212=CARTESIAN_POINT('Ctrl Pts',(5.64613369477574,-4.93794700987619,1.96343799118942));
#5213=CARTESIAN_POINT('Ctrl Pts',(5.68829012237593,-5.62472214856941,2.08693557381648));
#5214=CARTESIAN_POINT('Ctrl Pts',(5.73044654997612,-6.31149728726264,2.21043315644353));
#5215=CARTESIAN_POINT('Ctrl Pts',(5.77260297757631,-7.06520224831835,1.96173124287054));
#5216=CARTESIAN_POINT('Ctrl Pts',(5.8147594051765,-7.54360864801481,1.45375578994855));
#5217=CARTESIAN_POINT('Ctrl Pts',(5.85691583277669,-8.02201504771127,0.94578033702656));
#5218=CARTESIAN_POINT('Ctrl Pts',(5.89907226037688,-8.22512288604848,0.178531344755563));
#5219=CARTESIAN_POINT('Ctrl Pts',(5.94122868797708,-8.06070871907031,-0.499612980398527));
#5220=CARTESIAN_POINT('Ctrl Pts',(5.98338511557727,-7.89629455209214,-1.17775730555262));
#5221=CARTESIAN_POINT('Ctrl Pts',(6.02554154317746,-7.36435837979858,-1.76679696358982));
#5222=CARTESIAN_POINT('Ctrl Pts',(6.06769797077765,-6.70643192334511,-1.99927174058805));
#5223=CARTESIAN_POINT('Ctrl Pts',(6.10985439837784,-6.04850546689163,-2.23174651758629));
#5224=CARTESIAN_POINT('Ctrl Pts',(6.15201082597803,-5.26458872627824,-2.10765641354556));
#5225=CARTESIAN_POINT('Ctrl Pts',(6.19416725357822,-4.71062809031028,-1.68334596370979));
#5226=CARTESIAN_POINT('Ctrl Pts',(6.23309274271131,-4.19912391543011,-1.29155536985824));
#5227=CARTESIAN_POINT('Ctrl Pts',(6.2720182318444,-3.88367816056074,-0.643799722404717));
#5228=CARTESIAN_POINT('Ctrl Pts',(6.3109437209775,-3.88010896117177,0.000931372864572485));
#5229=CARTESIAN_POINT('Ctrl Pts',(6.0890562790225,-3.88123446329707,-0.00156260716336218));
#5230=CARTESIAN_POINT('Ctrl Pts',(6.08287937749084,-3.88038602380115,-0.104014736073326));
#5231=CARTESIAN_POINT('Ctrl Pts',(6.07670247595917,-3.8871808011753,-0.206353891857302));
#5232=CARTESIAN_POINT('Ctrl Pts',(6.07052557442751,-3.90200869710868,-0.307515583683664));
#5233=CARTESIAN_POINT('Ctrl Pts',(6.02836914682732,-4.00320686550659,-0.997928975499783));
#5234=CARTESIAN_POINT('Ctrl Pts',(5.98621271922713,-4.47857629044222,-1.63349776801118));
#5235=CARTESIAN_POINT('Ctrl Pts',(5.94405629162693,-5.11227003130558,-1.92563466002711));
#5236=CARTESIAN_POINT('Ctrl Pts',(5.90189986402674,-5.74596377216895,-2.21777155204305));
#5237=CARTESIAN_POINT('Ctrl Pts',(5.85974343642655,-6.53798182896006,-2.16647654356351));
#5238=CARTESIAN_POINT('Ctrl Pts',(5.81758700882636,-7.12869931732839,-1.7950407216212));
#5239=CARTESIAN_POINT('Ctrl Pts',(5.77543058122617,-7.71941680569672,-1.4236048996789));
#5240=CARTESIAN_POINT('Ctrl Pts',(5.73327415362598,-8.10883372564228,-0.732028264273839));
#5241=CARTESIAN_POINT('Ctrl Pts',(5.69111772602579,-8.12013085745316,-0.0343291201587056));
#5242=CARTESIAN_POINT('Ctrl Pts',(5.6489612984256,-8.13142798926403,0.663370023956428));
#5243=CARTESIAN_POINT('Ctrl Pts',(5.60680487082541,-7.76460533294022,1.36719167678164));
#5244=CARTESIAN_POINT('Ctrl Pts',(5.56464844322521,-7.18622292360526,1.75755754293546));
#5245=CARTESIAN_POINT('Ctrl Pts',(5.52249201562502,-6.60784051427029,2.14792340908928));
#5246=CARTESIAN_POINT('Ctrl Pts',(5.48033558802483,-5.81789835192417,2.22483348857171));
#5247=CARTESIAN_POINT('Ctrl Pts',(5.43817916042464,-5.17507873723095,1.95336587751692));
#5248=CARTESIAN_POINT('Ctrl Pts',(5.39602273282445,-4.53225912253772,1.68189826646213));
#5249=CARTESIAN_POINT('Ctrl Pts',(5.35386630522426,-4.03656205549739,1.06205296487013));
#5250=CARTESIAN_POINT('Ctrl Pts',(5.31170987762407,-3.91306447580689,0.375277842507117));
#5251=CARTESIAN_POINT('Ctrl Pts',(5.30415867809022,-3.89094317855098,0.252260398215228));
#5252=CARTESIAN_POINT('Ctrl Pts',(5.29660747855636,-3.88076396363212,0.127095499513492));
#5253=CARTESIAN_POINT('Ctrl Pts',(5.2890562790225,-3.88187782281943,0.00175000188907953));
#5254=CARTESIAN_POINT('Origin',(6.,-6.,0.));
#5255=CARTESIAN_POINT('',(4.4890562790225,-3.88640241446317,-5.40837461397714E-5));
#5256=CARTESIAN_POINT('',(4.71094372097749,-3.88380208938619,-0.00185818885717421));
#5257=CARTESIAN_POINT('',(6.,-3.883,2.59257727379495E-16));
#5258=CARTESIAN_POINT('Ctrl Pts',(4.71094372097749,-3.88380208938619,-0.00185818885717421));
#5259=CARTESIAN_POINT('Ctrl Pts',(4.74163086157564,-3.8881945038456,0.508719203379237));
#5260=CARTESIAN_POINT('Ctrl Pts',(4.77231800217378,-4.07403987422288,1.02216462871928));
#5261=CARTESIAN_POINT('Ctrl Pts',(4.80300514277192,-4.41013451264019,1.40301863392375));
#5262=CARTESIAN_POINT('Ctrl Pts',(4.84516157037211,-4.87184417392123,1.92621642895119));
#5263=CARTESIAN_POINT('Ctrl Pts',(4.8873179979723,-5.61710218276291,2.1991895235818));
#5264=CARTESIAN_POINT('Ctrl Pts',(4.92947442557249,-6.30751559099577,2.0979913527776));
#5265=CARTESIAN_POINT('Ctrl Pts',(4.97163085317269,-6.99792899922862,1.9967931819734));
#5266=CARTESIAN_POINT('Ctrl Pts',(5.01378728077288,-7.63349780685265,1.52142374573439));
#5267=CARTESIAN_POINT('Ctrl Pts',(5.05594370837307,-7.92563470581505,0.887729989802999));
#5268=CARTESIAN_POINT('Ctrl Pts',(5.09810013597325,-8.21777160477746,0.254036233871597));
#5269=CARTESIAN_POINT('Ctrl Pts',(5.14025656357344,-8.16647659507823,-0.537981841752198));
#5270=CARTESIAN_POINT('Ctrl Pts',(5.18241299117363,-7.7950407643039,-1.12869934416668));
#5271=CARTESIAN_POINT('Ctrl Pts',(5.22456941877382,-7.42360493352957,-1.71941684658117));
#5272=CARTESIAN_POINT('Ctrl Pts',(5.26672584637402,-6.73202828168015,-2.10883377578635));
#5273=CARTESIAN_POINT('Ctrl Pts',(5.30888227397421,-6.03432912097505,-2.12013090786587));
#5274=CARTESIAN_POINT('Ctrl Pts',(5.3510387015744,-5.33662996026994,-2.13142803994539));
#5275=CARTESIAN_POINT('Ctrl Pts',(5.3931951291746,-4.63280829070917,-1.76460537489925));
#5276=CARTESIAN_POINT('Ctrl Pts',(5.43535155677479,-4.24244241527317,-1.18622295181145));
#5277=CARTESIAN_POINT('Ctrl Pts',(5.46054894484236,-4.00911618220183,-0.840517037064096));
#5278=CARTESIAN_POINT('Ctrl Pts',(5.48574633290992,-3.88777492205943,-0.419229447894989));
#5279=CARTESIAN_POINT('Ctrl Pts',(5.51094372097749,-3.88587578853395,0.0010475127251217));
#5280=CARTESIAN_POINT('Ctrl Pts',(5.2890562790225,-3.88187782281943,0.00175000188907953));
#5281=CARTESIAN_POINT('Ctrl Pts',(5.25445105095617,-3.88698235634922,-0.572676552850085));
#5282=CARTESIAN_POINT('Ctrl Pts',(5.21984582288983,-4.12925905438439,-1.15089596655715));
#5283=CARTESIAN_POINT('Ctrl Pts',(5.18524059482349,-4.54624424461905,-1.54360861131074));
#5284=CARTESIAN_POINT('Ctrl Pts',(5.1430841672233,-5.05421968546235,-2.02201499963159));
#5285=CARTESIAN_POINT('Ctrl Pts',(5.10092773962312,-5.82146865948962,-2.22512283313927));
#5286=CARTESIAN_POINT('Ctrl Pts',(5.05877131202292,-6.49961296851871,-2.06070867007054));
#5287=CARTESIAN_POINT('Ctrl Pts',(5.01661488442273,-7.17775727754781,-1.89629450700181));
#5288=CARTESIAN_POINT('Ctrl Pts',(4.97445845682254,-7.76679692157875,-1.36435834735668));
#5289=CARTESIAN_POINT('Ctrl Pts',(4.93230202922235,-7.99927169304916,-0.706431906547451));
#5290=CARTESIAN_POINT('Ctrl Pts',(4.89014560162216,-8.23174646451957,-0.0485054657382238));
#5291=CARTESIAN_POINT('Ctrl Pts',(4.84798917402197,-8.10765636342946,0.735411256235103));
#5292=CARTESIAN_POINT('Ctrl Pts',(4.80583274642178,-7.68334592368299,1.28937187903092));
#5293=CARTESIAN_POINT('Ctrl Pts',(4.76367631882159,-7.25903548393652,1.84333250182674));
#5294=CARTESIAN_POINT('Ctrl Pts',(4.72151989122139,-6.53450470553368,2.16733702544503));
#5295=CARTESIAN_POINT('Ctrl Pts',(4.6793634636212,-5.83873509988996,2.11426747910681));
#5296=CARTESIAN_POINT('Ctrl Pts',(4.63720703602101,-5.14296549424625,2.0611979327686));
#5297=CARTESIAN_POINT('Ctrl Pts',(4.59505060842082,-4.47595706136166,1.63105431647387));
#5298=CARTESIAN_POINT('Ctrl Pts',(4.55289418082063,-4.14057263179942,1.01914827361007));
#5299=CARTESIAN_POINT('Ctrl Pts',(4.53161488022125,-3.97128062820059,0.71027645106943));
#5300=CARTESIAN_POINT('Ctrl Pts',(4.51033557962188,-3.88648402241563,0.355092876705326));
#5301=CARTESIAN_POINT('Ctrl Pts',(4.4890562790225,-3.88640241446317,-5.40837461397714E-5));
#5302=CARTESIAN_POINT('Origin',(6.,-6.,0.));
#5303=CARTESIAN_POINT('',(3.6890562790225,-3.88168480846505,-0.00170294642171713));
#5304=CARTESIAN_POINT('',(3.91094372097749,-3.87985545958303,0.000668395347130348));
#5305=CARTESIAN_POINT('',(6.,-3.883,2.59257727379495E-16));
#5306=CARTESIAN_POINT('Ctrl Pts',(3.91094372097749,-3.87985545958303,0.000668395347130348));
#5307=CARTESIAN_POINT('Ctrl Pts',(3.91320253504096,-3.87969984037501,0.0380697161946482));
#5308=CARTESIAN_POINT('Ctrl Pts',(3.91546134910444,-3.88060462371222,0.0754633564891892));
#5309=CARTESIAN_POINT('Ctrl Pts',(3.91772016316791,-3.88259359437381,0.112799239564616));
#5310=CARTESIAN_POINT('Ctrl Pts',(3.9598765907681,-3.91971391297379,0.809601812743023));
#5311=CARTESIAN_POINT('Ctrl Pts',(4.00203301836829,-4.33446812085637,1.48628693684409));
#5312=CARTESIAN_POINT('Ctrl Pts',(4.04418944596848,-4.9385323120656,1.83559796864891));
#5313=CARTESIAN_POINT('Ctrl Pts',(4.08634587356867,-5.54259650327483,2.18490900045374));
#5314=CARTESIAN_POINT('Ctrl Pts',(4.12850230116886,-6.33597067781071,2.20684593996233));
#5315=CARTESIAN_POINT('Ctrl Pts',(4.17065872876905,-6.95841419050323,1.8914480681416));
#5316=CARTESIAN_POINT('Ctrl Pts',(4.21281515636925,-7.58085770319576,1.57605019632088));
#5317=CARTESIAN_POINT('Ctrl Pts',(4.25497158396944,-8.03237055404493,0.923317513170838));
#5318=CARTESIAN_POINT('Ctrl Pts',(4.29712801156963,-8.10793815357666,0.229630781322297));
#5319=CARTESIAN_POINT('Ctrl Pts',(4.33928443916982,-8.18350575310838,-0.464055950526245));
#5320=CARTESIAN_POINT('Ctrl Pts',(4.38144086677001,-7.88312810132267,-1.19869673107329));
#5321=CARTESIAN_POINT('Ctrl Pts',(4.4235972943702,-7.34319511680599,-1.64071948645217));
#5322=CARTESIAN_POINT('Ctrl Pts',(4.46575372197039,-6.8032621322893,-2.08274224183105));
#5323=CARTESIAN_POINT('Ctrl Pts',(4.50791014957058,-6.02377381504164,-2.23214697204177));
#5324=CARTESIAN_POINT('Ctrl Pts',(4.55006657717077,-5.35866577743854,-2.02109474543042));
#5325=CARTESIAN_POINT('Ctrl Pts',(4.59222300477096,-4.69355773983544,-1.81004251881908));
#5326=CARTESIAN_POINT('Ctrl Pts',(4.63437943237116,-4.14282998187691,-1.23853333538567));
#5327=CARTESIAN_POINT('Ctrl Pts',(4.67653585997135,-3.95654675975784,-0.566067495956831));
#5328=CARTESIAN_POINT('Ctrl Pts',(4.6880051469734,-3.90586562144097,-0.383113100849401));
#5329=CARTESIAN_POINT('Ctrl Pts',(4.69947443397545,-3.8821604290332,-0.192685960170335));
#5330=CARTESIAN_POINT('Ctrl Pts',(4.71094372097749,-3.88380208938619,-0.00185818885717421));
#5331=CARTESIAN_POINT('Ctrl Pts',(4.4890562790225,-3.88640241446317,-5.40837461397714E-5));
#5332=CARTESIAN_POINT('Ctrl Pts',(4.46817915202169,-3.88632234888114,-0.348488853144316));
#5333=CARTESIAN_POINT('Ctrl Pts',(4.44730202502087,-3.96778535574421,-0.696888379539397));
#5334=CARTESIAN_POINT('Ctrl Pts',(4.42642489802006,-4.1309988177518,-1.00148286154596));
#5335=CARTESIAN_POINT('Ctrl Pts',(4.38426847041987,-4.46056985950631,-1.61653948440537));
#5336=CARTESIAN_POINT('Ctrl Pts',(4.34211204281968,-5.12347236925522,-2.05298426069133));
#5337=CARTESIAN_POINT('Ctrl Pts',(4.29995561521949,-5.81870785793641,-2.11264443303735));
#5338=CARTESIAN_POINT('Ctrl Pts',(4.2577991876193,-6.5139433466176,-2.17230460538337));
#5339=CARTESIAN_POINT('Ctrl Pts',(4.2156427600191,-7.24151181423107,-1.85518017378945));
#5340=CARTESIAN_POINT('Ctrl Pts',(4.17348633241891,-7.67105245172811,-1.3052651243282));
#5341=CARTESIAN_POINT('Ctrl Pts',(4.13132990481872,-8.10059308922514,-0.755350074866954));
#5342=CARTESIAN_POINT('Ctrl Pts',(4.08917347721853,-8.23210589660575,0.0273555924616259));
#5343=CARTESIAN_POINT('Ctrl Pts',(4.04701704961834,-8.00587597502505,0.687455390575113));
#5344=CARTESIAN_POINT('Ctrl Pts',(4.00486062201815,-7.77964605344434,1.3475551886886));
#5345=CARTESIAN_POINT('Ctrl Pts',(3.96270419441796,-7.19567340290233,1.885049117587));
#5346=CARTESIAN_POINT('Ctrl Pts',(3.92054776681776,-6.51911750444087,2.05588189296251));
#5347=CARTESIAN_POINT('Ctrl Pts',(3.87839133921757,-5.84256160597942,2.22671466833802));
#5348=CARTESIAN_POINT('Ctrl Pts',(3.83623491161738,-5.07342245959854,2.03088629019065));
#5349=CARTESIAN_POINT('Ctrl Pts',(3.79407848401719,-4.56093651792191,1.55731488008976));
#5350=CARTESIAN_POINT('Ctrl Pts',(3.75907108235229,-4.13535963133093,1.16405327055198));
#5351=CARTESIAN_POINT('Ctrl Pts',(3.7240636806874,-3.88676871644664,0.579262315211952));
#5352=CARTESIAN_POINT('Ctrl Pts',(3.6890562790225,-3.88168480846505,-0.00170294642171713));
#5353=CARTESIAN_POINT('Origin',(6.,-6.,0.));
#5354=CARTESIAN_POINT('',(2.8890562790225,-3.88141756531907,0.00162515511074018));
#5355=CARTESIAN_POINT('',(3.11094372097749,-3.88560636234646,0.00125599444870333));
#5356=CARTESIAN_POINT('',(6.,-3.883,2.59257727379495E-16));
#5357=CARTESIAN_POINT('Ctrl Pts',(3.11094372097749,-3.88560636234646,0.00125599444870333));
#5358=CARTESIAN_POINT('Ctrl Pts',(3.12693063610648,-3.8841502733519,0.267822688839656));
#5359=CARTESIAN_POINT('Ctrl Pts',(3.14291755123548,-3.93091517346986,0.533897324592317));
#5360=CARTESIAN_POINT('Ctrl Pts',(3.15890446636447,-4.02825317932317,0.779966685220892));
#5361=CARTESIAN_POINT('Ctrl Pts',(3.20106089396466,-4.28492700059471,1.4288351568594));
#5362=CARTESIAN_POINT('Ctrl Pts',(3.24321732156485,-4.89325670544289,1.93859861215253));
#5363=CARTESIAN_POINT('Ctrl Pts',(3.28537374916504,-5.57702321297396,2.07779310633982));
#5364=CARTESIAN_POINT('Ctrl Pts',(3.32753017676523,-6.26078972050503,2.21698760052711));
#5365=CARTESIAN_POINT('Ctrl Pts',(3.36968660436542,-7.01999303071899,1.98561313360857));
#5366=CARTESIAN_POINT('Ctrl Pts',(3.41184303196561,-7.50990817134806,1.48872793656901));
#5367=CARTESIAN_POINT('Ctrl Pts',(3.45399945956581,-7.99982331197713,0.991842739529444));
#5368=CARTESIAN_POINT('Ctrl Pts',(3.496155887166,-8.22045028302133,0.229446812368861));
#5369=CARTESIAN_POINT('Ctrl Pts',(3.53831231476619,-8.07161087736646,-0.452285228363516));
#5370=CARTESIAN_POINT('Ctrl Pts',(3.58046874236638,-7.9227714717116,-1.13401726909589));
#5371=CARTESIAN_POINT('Ctrl Pts',(3.62262516996657,-7.40446568935766,-1.73508542340006));
#5372=CARTESIAN_POINT('Ctrl Pts',(3.66478159756676,-6.75203621653659,-1.98256780062233));
#5373=CARTESIAN_POINT('Ctrl Pts',(3.70693802516695,-6.09960674371551,-2.2300501778446));
#5374=CARTESIAN_POINT('Ctrl Pts',(3.74909445276714,-5.31305358042728,-2.12394677798495));
#5375=CARTESIAN_POINT('Ctrl Pts',(3.79125088036734,-4.74952021344186,-1.71243506692724));
#5376=CARTESIAN_POINT('Ctrl Pts',(3.83114849390406,-4.21618193572383,-1.32297286274512));
#5377=CARTESIAN_POINT('Ctrl Pts',(3.87104610744078,-3.88260417410584,-0.659954127360146));
#5378=CARTESIAN_POINT('Ctrl Pts',(3.91094372097749,-3.87985545958303,0.000668395347130348));
#5379=CARTESIAN_POINT('Ctrl Pts',(3.6890562790225,-3.88168480846505,-0.00170294642171713));
#5380=CARTESIAN_POINT('Ctrl Pts',(3.68190725308721,-3.88064659973533,-0.120344591485258));
#5381=CARTESIAN_POINT('Ctrl Pts',(3.67475822715191,-3.8897635201934,-0.238826691185751));
#5382=CARTESIAN_POINT('Ctrl Pts',(3.66760920121662,-3.90960209601946,-0.355485504963693));
#5383=CARTESIAN_POINT('Ctrl Pts',(3.62545277361643,-4.02658635276603,-1.04340003786182));
#5384=CARTESIAN_POINT('Ctrl Pts',(3.58329634601624,-4.51638760323151,-1.66791466160366));
#5385=CARTESIAN_POINT('Ctrl Pts',(3.54113991841605,-5.1566059708734,-1.94546134706676));
#5386=CARTESIAN_POINT('Ctrl Pts',(3.49898349081586,-5.79682433851529,-2.22300803252987));
#5387=CARTESIAN_POINT('Ctrl Pts',(3.45682706321567,-6.58745982333359,-2.15358677971423));
#5388=CARTESIAN_POINT('Ctrl Pts',(3.41467063561547,-7.16951531363361,-1.76871910496289));
#5389=CARTESIAN_POINT('Ctrl Pts',(3.37251420801528,-7.75157080393361,-1.38385143021156));
#5390=CARTESIAN_POINT('Ctrl Pts',(3.33035778041509,-8.12504629971534,-0.683537333524543));
#5391=CARTESIAN_POINT('Ctrl Pts',(3.2882013528149,-8.12036096779767,0.0142375360740912));
#5392=CARTESIAN_POINT('Ctrl Pts',(3.24604492521471,-8.11567563588001,0.712012405672736));
#5393=CARTESIAN_POINT('Ctrl Pts',(3.20388849761452,-7.73282947626296,1.40724804818299));
#5394=CARTESIAN_POINT('Ctrl Pts',(3.16173207001432,-7.14565817952281,1.78426474421204));
#5395=CARTESIAN_POINT('Ctrl Pts',(3.11957564241413,-6.55848688278268,2.16128144024109));
#5396=CARTESIAN_POINT('Ctrl Pts',(3.07741921481394,-5.76699044891946,2.22007918978893));
#5397=CARTESIAN_POINT('Ctrl Pts',(3.03526278721375,-5.13055691347015,1.93396020110993));
#5398=CARTESIAN_POINT('Ctrl Pts',(2.99310635961356,-4.49412337802086,1.64784121243092));
#5399=CARTESIAN_POINT('Ctrl Pts',(2.95094993201337,-4.01275274098548,1.01680548552507));
#5400=CARTESIAN_POINT('Ctrl Pts',(2.90879350441318,-3.9050168620548,0.327382029349999));
#5401=CARTESIAN_POINT('Ctrl Pts',(2.90221442928295,-3.88820323523547,0.219788265529837));
#5402=CARTESIAN_POINT('Ctrl Pts',(2.89563535415273,-3.88048977537532,0.110772422866118));
#5403=CARTESIAN_POINT('Ctrl Pts',(2.8890562790225,-3.88141756531907,0.00162515511074018));
#5404=CARTESIAN_POINT('Origin',(6.,-6.,0.));
#5405=CARTESIAN_POINT('',(2.0890562790225,-3.88638481832281,0.000206967542925318));
#5406=CARTESIAN_POINT('',(2.31094372097749,-3.88425079107578,-0.00178855544584995));
#5407=CARTESIAN_POINT('',(6.,-3.883,2.59257727379495E-16));
#5408=CARTESIAN_POINT('Ctrl Pts',(2.31094372097749,-3.88425079107578,-0.00178855544584995));
#5409=CARTESIAN_POINT('Ctrl Pts',(2.34065873717201,-3.88827746358585,0.49288078299178));
#5410=CARTESIAN_POINT('Ctrl Pts',(2.37037375336652,-4.06150217415285,0.990091561638185));
#5411=CARTESIAN_POINT('Ctrl Pts',(2.40008876956103,-4.37841802272573,1.36623769466599));
#5412=CARTESIAN_POINT('Ctrl Pts',(2.44224519716122,-4.82802370149306,1.89987284802682));
#5413=CARTESIAN_POINT('Ctrl Pts',(2.48440162476141,-5.56683427812707,2.18984308956855));
#5414=CARTESIAN_POINT('Ctrl Pts',(2.5265580523616,-6.25938433842444,2.10448409909473));
#5415=CARTESIAN_POINT('Ctrl Pts',(2.56871447996179,-6.95193439872182,2.01912510862091));
#5416=CARTESIAN_POINT('Ctrl Pts',(2.61087090756198,-7.59822394268257,1.55843688613156));
#5417=CARTESIAN_POINT('Ctrl Pts',(2.65302733516218,-7.9047977871553,0.931600206785907));
#5418=CARTESIAN_POINT('Ctrl Pts',(2.69518376276237,-8.21137163162803,0.304763527440254));
#5419=CARTESIAN_POINT('Ctrl Pts',(2.73734019036256,-8.17822977661274,-0.488221608761689));
#5420=CARTESIAN_POINT('Ctrl Pts',(2.77949661796275,-7.82042066249784,-1.0872912055028));
#5421=CARTESIAN_POINT('Ctrl Pts',(2.82165304556294,-7.46261154838294,-1.6863608022439));
#5422=CARTESIAN_POINT('Ctrl Pts',(2.86380947316313,-6.78013517516843,-2.09151485952416));
#5423=CARTESIAN_POINT('Ctrl Pts',(2.90596590076332,-6.08287776867917,-2.11878852909447));
#5424=CARTESIAN_POINT('Ctrl Pts',(2.94812232836351,-5.3856203621899,-2.14606219866477));
#5425=CARTESIAN_POINT('Ctrl Pts',(2.9902787559637,-4.67358192242587,-1.7954554805251));
#5426=CARTESIAN_POINT('Ctrl Pts',(3.0324351835639,-4.2700716713913,-1.22616537746331));
#5427=CARTESIAN_POINT('Ctrl Pts',(3.0586046960351,-4.01958397241328,-0.872766256619923));
#5428=CARTESIAN_POINT('Ctrl Pts',(3.08477420850629,-3.88798988279394,-0.435095883132698));
#5429=CARTESIAN_POINT('Ctrl Pts',(3.11094372097749,-3.88560636234646,0.00125599444870333));
#5430=CARTESIAN_POINT('Ctrl Pts',(2.8890562790225,-3.88141756531907,0.00162515511074018));
#5431=CARTESIAN_POINT('Ctrl Pts',(2.85347892655253,-3.88643473098346,-0.588605346776316));
#5432=CARTESIAN_POINT('Ctrl Pts',(2.81790157408257,-4.14414542594115,-1.18267907400726));
#5433=CARTESIAN_POINT('Ctrl Pts',(2.78232422161261,-4.58197906344156,-1.5764992762549));
#5434=CARTESIAN_POINT('Ctrl Pts',(2.74016779401242,-5.10077826458496,-2.04314594024041));
#5435=CARTESIAN_POINT('Ctrl Pts',(2.69801136641223,-5.87247778769773,-2.22862808276713));
#5436=CARTESIAN_POINT('Ctrl Pts',(2.65585493881203,-6.54667861130499,-2.04872541582711));
#5437=CARTESIAN_POINT('Ctrl Pts',(2.61369851121184,-7.22087943491225,-1.86882274888709));
#5438=CARTESIAN_POINT('Ctrl Pts',(2.57154208361165,-7.797581559014,-1.32353527248033));
#5439=CARTESIAN_POINT('Ctrl Pts',(2.52938565601146,-8.01492676931713,-0.660457007976325));
#5440=CARTESIAN_POINT('Ctrl Pts',(2.48722922841127,-8.23227197962026,0.00262125652767495));
#5441=CARTESIAN_POINT('Ctrl Pts',(2.44507280081108,-8.09026027612478,0.783490309128911));
#5442=CARTESIAN_POINT('Ctrl Pts',(2.40291637321089,-7.65337370033519,1.32758757464938));
#5443=CARTESIAN_POINT('Ctrl Pts',(2.3607599456107,-7.2164871245456,1.87168484016984));
#5444=CARTESIAN_POINT('Ctrl Pts',(2.3186035180105,-6.48472567646189,2.17901031860954));
#5445=CARTESIAN_POINT('Ctrl Pts',(2.27644709041031,-5.79035403900129,2.11001939707077));
#5446=CARTESIAN_POINT('Ctrl Pts',(2.23429066281012,-5.09598240154068,2.04102847553199));
#5447=CARTESIAN_POINT('Ctrl Pts',(2.19213423520993,-4.43900057470318,1.59572115401476));
#5448=CARTESIAN_POINT('Ctrl Pts',(2.14997780760974,-4.11771868783986,0.976294242006309));
#5449=CARTESIAN_POINT('Ctrl Pts',(2.129670631414,-3.96295396377662,0.67791005343511));
#5450=CARTESIAN_POINT('Ctrl Pts',(2.10936345521825,-3.88608659904271,0.339122353597826));
#5451=CARTESIAN_POINT('Ctrl Pts',(2.0890562790225,-3.88638481832281,0.000206967542925318));
#5452=CARTESIAN_POINT('Origin',(6.,-6.,0.));
#5453=CARTESIAN_POINT('',(1.2890562790225,-3.88215585431528,-0.00180833227560233));
#5454=CARTESIAN_POINT('',(1.51094372097749,-3.87968050865492,0.000387557652718817));
#5455=CARTESIAN_POINT('',(6.,-3.883,2.59257727379495E-16));
#5456=CARTESIAN_POINT('Ctrl Pts',(1.51094372097749,-3.87968050865492,0.000387557652718817));
#5457=CARTESIAN_POINT('Ctrl Pts',(1.51223041063733,-3.87962643184165,0.0216877999309881));
#5458=CARTESIAN_POINT('Ctrl Pts',(1.51351710029718,-3.8799198812182,0.0429865156964861));
#5459=CARTESIAN_POINT('Ctrl Pts',(1.51480378995702,-3.88056546385779,0.0642745521975925));
#5460=CARTESIAN_POINT('Ctrl Pts',(1.55696021755721,-3.90171699608445,0.761744655143333));
#5461=CARTESIAN_POINT('Ctrl Pts',(1.5991166451574,-4.30086437795335,1.44775115029935));
#5462=CARTESIAN_POINT('Ctrl Pts',(1.64127307275759,-4.89676984071834,1.81080544827727));
#5463=CARTESIAN_POINT('Ctrl Pts',(1.68342950035778,-5.49267530348333,2.17385974625519));
#5464=CARTESIAN_POINT('Ctrl Pts',(1.72558592795797,-6.2853388471444,2.21396184705501));
#5465=CARTESIAN_POINT('Ctrl Pts',(1.76774235555817,-6.91484266441608,1.91290265527438));
#5466=CARTESIAN_POINT('Ctrl Pts',(1.80989878315836,-7.54434648168775,1.61184346349375));
#5467=CARTESIAN_POINT('Ctrl Pts',(1.85205521075855,-8.01069057257003,0.969622979132674));
#5468=CARTESIAN_POINT('Ctrl Pts',(1.89421163835874,-8.10212596526366,0.277848924816985));
#5469=CARTESIAN_POINT('Ctrl Pts',(1.93636806595893,-8.19356135795729,-0.413925129498698));
#5470=CARTESIAN_POINT('Ctrl Pts',(1.97852449355912,-7.91008805246229,-1.15525275376899));
#5471=CARTESIAN_POINT('Ctrl Pts',(2.02068092115931,-7.38042040080226,-1.60952571148568));
#5472=CARTESIAN_POINT('Ctrl Pts',(2.0628373487595,-6.85075274914223,-2.06379866920236));
#5473=CARTESIAN_POINT('Ctrl Pts',(2.10499377635969,-6.07489075131718,-2.23101696036544));
#5474=CARTESIAN_POINT('Ctrl Pts',(2.14715020395988,-5.40512342384882,-2.03525316220135));
#5475=CARTESIAN_POINT('Ctrl Pts',(2.18930663156007,-4.73535609638045,-1.83948936403726));
#5476=CARTESIAN_POINT('Ctrl Pts',(2.23146305916027,-4.17168343926878,-1.280743476546));
#5477=CARTESIAN_POINT('Ctrl Pts',(2.27361948676046,-3.97004750116327,-0.6127205002104));
#5478=CARTESIAN_POINT('Ctrl Pts',(2.28606089816614,-3.9105397154483,-0.415570287297211));
#5479=CARTESIAN_POINT('Ctrl Pts',(2.29850230957181,-3.88256485932444,-0.20890218139817));
#5480=CARTESIAN_POINT('Ctrl Pts',(2.31094372097749,-3.88425079107578,-0.00178855544584995));
#5481=CARTESIAN_POINT('Ctrl Pts',(2.0890562790225,-3.88638481832281,0.000206967542925318));
#5482=CARTESIAN_POINT('Ctrl Pts',(2.06720702761806,-3.88670568361505,-0.364444789223636));
#5483=CARTESIAN_POINT('Ctrl Pts',(2.04535777621361,-3.97635662359167,-0.729244360841879));
#5484=CARTESIAN_POINT('Ctrl Pts',(2.02350852480917,-4.15442617570082,-1.04402620399982));
#5485=CARTESIAN_POINT('Ctrl Pts',(1.98135209720898,-4.49799749731423,-1.65137323549784));
#5486=CARTESIAN_POINT('Ctrl Pts',(1.93919566960879,-5.17072208743017,-2.0725207959942));
#5487=CARTESIAN_POINT('Ctrl Pts',(1.8970392420086,-5.8671416077804,-2.11624232759768));
#5488=CARTESIAN_POINT('Ctrl Pts',(1.8548828144084,-6.56356112813062,-2.15996385920116));
#5489=CARTESIAN_POINT('Ctrl Pts',(1.81272638680821,-7.28367557871513,-1.82625936191177));
#5490=CARTESIAN_POINT('Ctrl Pts',(1.77056995920802,-7.70050877250907,-1.26665057227176));
#5491=CARTESIAN_POINT('Ctrl Pts',(1.72841353160783,-8.11734196630301,-0.707041782631743));
#5492=CARTESIAN_POINT('Ctrl Pts',(1.68625710400764,-8.23089390330638,0.0784712993588993));
#5493=CARTESIAN_POINT('Ctrl Pts',(1.64410067640745,-7.98960494718644,0.733216263819768));
#5494=CARTESIAN_POINT('Ctrl Pts',(1.60194424880726,-7.74831599106649,1.38796122828064));
#5495=CARTESIAN_POINT('Ctrl Pts',(1.55978782120707,-7.15218614182322,1.91193807521173));
#5496=CARTESIAN_POINT('Ctrl Pts',(1.51763139360688,-6.47189514288099,2.06723137262971));
#5497=CARTESIAN_POINT('Ctrl Pts',(1.47547496600669,-5.79160414393876,2.22252467004768));
#5498=CARTESIAN_POINT('Ctrl Pts',(1.4333185384065,-5.02715199529757,2.00913441795253));
#5499=CARTESIAN_POINT('Ctrl Pts',(1.3911621108063,-4.52564668340792,1.52394857057864));
#5500=CARTESIAN_POINT('Ctrl Pts',(1.35712683354504,-4.12075297419606,1.13223049154154));
#5501=CARTESIAN_POINT('Ctrl Pts',(1.32309155628377,-3.88725457516647,0.563349260688335));
#5502=CARTESIAN_POINT('Ctrl Pts',(1.2890562790225,-3.88215585431528,-0.00180833227560233));
#5503=CARTESIAN_POINT('Origin',(6.,-6.,0.));
#5504=CARTESIAN_POINT('',(0.4890562790225,-3.88098062526521,0.00140302826277638));
#5505=CARTESIAN_POINT('',(0.710943720977493,-3.88529148023119,0.00143577679747337));
#5506=CARTESIAN_POINT('',(6.,-3.883,2.59257727379495E-16));
#5507=CARTESIAN_POINT('',(0.,-7.61992569438872,1.36291222925734));
#5508=CARTESIAN_POINT('Ctrl Pts',(0.4890562790225,-3.88098062526521,0.00140302826277638));
#5509=CARTESIAN_POINT('Ctrl Pts',(0.452506802148906,-3.88578409771184,-0.604476981624192));
#5510=CARTESIAN_POINT('Ctrl Pts',(0.415957325275312,-4.15953906766724,-1.21398517371684));
#5511=CARTESIAN_POINT('Ctrl Pts',(0.379407848401718,-4.61847166921745,-1.60833849276868));
#5512=CARTESIAN_POINT('Ctrl Pts',(0.337251420801527,-5.14780780876139,-2.06318842676363));
#5513=CARTESIAN_POINT('Ctrl Pts',(0.295094993201337,-5.92349464593687,-2.23180749898577));
#5514=CARTESIAN_POINT('Ctrl Pts',(0.252938565601146,-6.59343701884389,-2.03607518357452));
#5515=CARTESIAN_POINT('Ctrl Pts',(0.210782138000955,-7.26337939175092,-1.84034286816327));
#5516=CARTESIAN_POINT('Ctrl Pts',(0.168625710400764,-7.82757730038949,-1.28025916511862));
#5517=CARTESIAN_POINT('Ctrl Pts',(0.126469282800573,-8.02952750753659,-0.613533042485344));
#5518=CARTESIAN_POINT('Ctrl Pts',(0.0843128552003817,-8.23147771468369,
0.0531930801479328));
#5519=CARTESIAN_POINT('Ctrl Pts',(0.0421564276001906,-8.07118022033932,
0.826561622369841));
#5520=CARTESIAN_POINT('Ctrl Pts',(-4.10547488943358E-16,-7.61992569438872,
1.36291222925734));
#5521=CARTESIAN_POINT('',(2.70473896144179E-15,-4.37709039209165,1.36522613564372));
#5522=CARTESIAN_POINT('Origin',(0.,-6.,0.));
#5523=CARTESIAN_POINT('Ctrl Pts',(1.80411241501588E-15,-4.37708920932832,
1.36522705282968));
#5524=CARTESIAN_POINT('Ctrl Pts',(0.0412138930502395,-4.8171154211057,1.88675622363143));
#5525=CARTESIAN_POINT('Ctrl Pts',(0.0824277861004773,-5.53232983704421,
2.17777740054626));
#5526=CARTESIAN_POINT('Ctrl Pts',(0.123641679150715,-6.21123416498923,2.10968102048252));
#5527=CARTESIAN_POINT('Ctrl Pts',(0.165798106750906,-6.90566458711858,2.04002732112213));
#5528=CARTESIAN_POINT('Ctrl Pts',(0.207954534351097,-7.56210515530846,1.59464268056525));
#5529=CARTESIAN_POINT('Ctrl Pts',(0.250110961951288,-7.88289993702619,0.975083106675219));
#5530=CARTESIAN_POINT('Ctrl Pts',(0.292267389551479,-8.20369471874392,0.355523532785185));
#5531=CARTESIAN_POINT('Ctrl Pts',(0.33442381715167,-8.18884371398951,-0.438210974438008));
#5532=CARTESIAN_POINT('Ctrl Pts',(0.376580244751861,-7.84487777104374,-1.04536577050709));
#5533=CARTESIAN_POINT('Ctrl Pts',(0.418736672352052,-7.50091182809796,-1.65252056657617));
#5534=CARTESIAN_POINT('Ctrl Pts',(0.460893099952243,-6.82783094696082,-2.07309565149114));
#5535=CARTESIAN_POINT('Ctrl Pts',(0.503049527552434,-6.13136608707291,-2.11630681992121));
#5536=CARTESIAN_POINT('Ctrl Pts',(0.545205955152625,-5.43490122718498,-2.15951798835128));
#5537=CARTESIAN_POINT('Ctrl Pts',(0.587362382752816,-4.71505238854628,-1.82536524029645));
#5538=CARTESIAN_POINT('Ctrl Pts',(0.629518810353007,-4.2986172899441,-1.26547903592209));
#5539=CARTESIAN_POINT('Ctrl Pts',(0.656660447227835,-4.03050324727928,-0.905006649730477));
#5540=CARTESIAN_POINT('Ctrl Pts',(0.683802084102664,-3.8881599727947,-0.450963450951839));
#5541=CARTESIAN_POINT('Ctrl Pts',(0.710943720977493,-3.88529148023119,0.00143577679747337));
#5542=CARTESIAN_POINT('Origin',(-1.7667098902285,-6.,0.));
#5543=CARTESIAN_POINT('',(10.5667098902285,-3.44386948695903,0.000692352191159762));
#5544=CARTESIAN_POINT('',(10.6332901097715,-3.43705236943178,-0.00151513564181791));
#5545=CARTESIAN_POINT('',(-1.7667098902285,-3.44,1.9679933794996E-13));
#5546=CARTESIAN_POINT('',(11.,-8.47299490241841,0.661737268568548));
#5547=CARTESIAN_POINT('Ctrl Pts',(10.6332901097715,-3.43705236943178,-0.00151513564181784));
#5548=CARTESIAN_POINT('Ctrl Pts',(10.6712138846473,-3.44184769772038,0.758560196074207));
#5549=CARTESIAN_POINT('Ctrl Pts',(10.7512940871233,-4.19985142761009,2.37288109075158));
#5550=CARTESIAN_POINT('Ctrl Pts',(10.8735307171994,-6.94276063434935,2.8696483143193));
#5551=CARTESIAN_POINT('Ctrl Pts',(10.9578435723998,-8.2538964667147,1.48053551427594));
#5552=CARTESIAN_POINT('Ctrl Pts',(11.,-8.47299490241841,0.661737268568548));
#5553=CARTESIAN_POINT('',(11.,-8.47735530983487,-0.663092355832106));
#5554=CARTESIAN_POINT('Origin',(11.,-6.,0.));
#5555=CARTESIAN_POINT('Ctrl Pts',(10.5667098902285,-3.44386948695903,0.000692352191160109));
#5556=CARTESIAN_POINT('Ctrl Pts',(10.5856131785684,-3.4429055464256,0.382134963423751));
#5557=CARTESIAN_POINT('Ctrl Pts',(10.6466728945085,-3.70136760183046,1.61303222180456));
#5558=CARTESIAN_POINT('Ctrl Pts',(10.7498890380487,-5.60254915406858,2.99513384905324));
#5559=CARTESIAN_POINT('Ctrl Pts',(10.8754157862993,-8.27098793310559,1.97617764674277));
#5560=CARTESIAN_POINT('Ctrl Pts',(10.9587861069498,-8.68954097008596,0.134309514573586));
#5561=CARTESIAN_POINT('Ctrl Pts',(11.,-8.4773570382127,-0.663092892961434));
#5562=CARTESIAN_POINT('Origin',(-1.7667098902285,-6.,0.));
#5563=CARTESIAN_POINT('',(9.76670989022852,-3.43982213984121,-0.00227838982848949));
#5564=CARTESIAN_POINT('',(9.8332901097715,-3.43981019619369,0.0022738699535656));
#5565=CARTESIAN_POINT('',(-1.7667098902285,-3.44,1.9679933794996E-13));
#5566=CARTESIAN_POINT('Ctrl Pts',(9.8332901097715,-3.43981019619369,0.00227386995356616));
#5567=CARTESIAN_POINT('Ctrl Pts',(9.84278555811261,-3.43807597231295,0.193098490195483));
#5568=CARTESIAN_POINT('Ctrl Pts',(9.89443743405392,-3.54439859556582,1.22920418622825));
#5569=CARTESIAN_POINT('Ctrl Pts',(9.98824573759542,-4.95320971865872,2.83433293290292));
#5570=CARTESIAN_POINT('Ctrl Pts',(10.114715020396,-7.80326121920459,2.4243168480084));
#5571=CARTESIAN_POINT('Ctrl Pts',(10.2411843031966,-9.01549208379667,-0.187132795629694));
#5572=CARTESIAN_POINT('Ctrl Pts',(10.3676535859971,-7.48974052152724,-2.62891886486708));
#5573=CARTESIAN_POINT('Ctrl Pts',(10.4941228687977,-4.61024985438304,-2.68279494587922));
#5574=CARTESIAN_POINT('Ctrl Pts',(10.5826683767225,-3.47900431032775,-1.0154815268328));
#5575=CARTESIAN_POINT('Ctrl Pts',(10.6290574570471,-3.4365171653438,-0.0863467467902525));
#5576=CARTESIAN_POINT('Ctrl Pts',(10.6332901097715,-3.43705236943178,-0.00151513564181784));
#5577=CARTESIAN_POINT('Ctrl Pts',(9.76670989022852,-3.43982213984121,-0.00227838982848942));
#5578=CARTESIAN_POINT('Ctrl Pts',(9.79934127963391,-3.44577993040473,0.653508085119705));
#5579=CARTESIAN_POINT('Ctrl Pts',(9.8741290966395,-4.03530828415894,2.16602520880728));
#5580=CARTESIAN_POINT('Ctrl Pts',(9.99107334124527,-6.57463978426254,2.96628135292037));
#5581=CARTESIAN_POINT('Ctrl Pts',(10.1175426240459,-8.79891519692859,1.13796717239844));
#5582=CARTESIAN_POINT('Ctrl Pts',(10.2440119068464,-8.4815071817026,-1.72375621929785));
#5583=CARTESIAN_POINT('Ctrl Pts',(10.370481189647,-5.91044069571119,-3.02010639410425));
#5584=CARTESIAN_POINT('Ctrl Pts',(10.4780471841077,-3.79308023070163,-1.7899877019098));
#5585=CARTESIAN_POINT('Ctrl Pts',(10.5434567509682,-3.44505524062577,-0.468524325845745));
#5586=CARTESIAN_POINT('Ctrl Pts',(10.5667098902285,-3.44386948695903,0.000692352191160109));
#5587=CARTESIAN_POINT('Origin',(-1.7667098902285,-6.,0.));
#5588=CARTESIAN_POINT('',(8.96670989022851,-3.43689094140915,0.00141529279526265));
#5589=CARTESIAN_POINT('',(9.0332901097715,-3.44394015329315,-0.000687443883765837));
#5590=CARTESIAN_POINT('',(-1.7667098902285,-3.44,1.9679933794996E-13));
#5591=CARTESIAN_POINT('Ctrl Pts',(9.0332901097715,-3.44394015329315,-0.0006874438837658));
#5592=CARTESIAN_POINT('Ctrl Pts',(9.05651365917813,-3.44507664468085,0.467936431888932));
#5593=CARTESIAN_POINT('Ctrl Pts',(9.12189363618495,-3.79229911794252,1.7887946585363));
#5594=CARTESIAN_POINT('Ctrl Pts',(9.22943004079198,-5.90841299622533,3.0200385622781));
#5595=CARTESIAN_POINT('Ctrl Pts',(9.35589932359255,-8.48026503905977,1.72548764368831));
#5596=CARTESIAN_POINT('Ctrl Pts',(9.48236860639313,-8.79972666043973,-1.1360152599871));
#5597=CARTESIAN_POINT('Ctrl Pts',(9.60883788919369,-6.57670152087419,-2.96588225471199));
#5598=CARTESIAN_POINT('Ctrl Pts',(9.72581172365316,-4.03617235544237,-2.1671874966241));
#5599=CARTESIAN_POINT('Ctrl Pts',(9.80062913051242,-3.44577531212764,-0.654095238691659));
#5600=CARTESIAN_POINT('Ctrl Pts',(9.8332901097715,-3.43981019619369,0.00227386995356616));
#5601=CARTESIAN_POINT('Ctrl Pts',(8.96670989022851,-3.43689094140915,0.00141529279526262));
#5602=CARTESIAN_POINT('Ctrl Pts',(8.97091295309924,-3.43632903198528,0.0856328825033177));
#5603=CARTESIAN_POINT('Ctrl Pts',(9.01727244357015,-3.4781806728961,1.01398188137752));
#5604=CARTESIAN_POINT('Ctrl Pts',(9.10578836164126,-4.60885239449141,2.68211248963539));
#5605=CARTESIAN_POINT('Ctrl Pts',(9.23225764444184,-7.48766074739694,2.6298070334431));
#5606=CARTESIAN_POINT('Ctrl Pts',(9.3587269272424,-9.01548944052047,0.189313422437645));
#5607=CARTESIAN_POINT('Ctrl Pts',(9.48519621004299,-7.80488452630467,-2.42309995159429));
#5608=CARTESIAN_POINT('Ctrl Pts',(9.61166549284354,-4.95521961969974,-2.83504085634446));
#5609=CARTESIAN_POINT('Ctrl Pts',(9.70550338623873,-3.54480869101683,-1.23041260512691));
#5610=CARTESIAN_POINT('Ctrl Pts',(9.75718485203372,-3.43808307252877,-0.193701168181872));
#5611=CARTESIAN_POINT('Ctrl Pts',(9.76670989022852,-3.43982213984121,-0.00227838982848942));
#5612=CARTESIAN_POINT('Origin',(-1.7667098902285,-6.,0.));
#5613=CARTESIAN_POINT('',(8.16670989022851,-3.44373997328344,0.000990877584209626));
#5614=CARTESIAN_POINT('',(8.2332901097715,-3.43735861323487,-0.00167649580848317));
#5615=CARTESIAN_POINT('',(-1.7667098902285,-3.44,1.9679933794996E-13));
#5616=CARTESIAN_POINT('Ctrl Pts',(8.2332901097715,-3.43735861323486,-0.0016764958084832));
#5617=CARTESIAN_POINT('Ctrl Pts',(8.27024176024366,-3.44299005962199,0.739085989948098));
#5618=CARTESIAN_POINT('Ctrl Pts',(8.349349838316,-4.16926208645861,2.33458270048732));
#5619=CARTESIAN_POINT('Ctrl Pts',(8.47061434398855,-6.87308161737107,2.89253294855792));
#5620=CARTESIAN_POINT('Ctrl Pts',(8.59708362678911,-8.90008601701954,0.847655336961254));
#5621=CARTESIAN_POINT('Ctrl Pts',(8.72355290958969,-8.29345566941167,-1.96699747432336));
#5622=CARTESIAN_POINT('Ctrl Pts',(8.85002219239025,-5.60408579766473,-2.99537486433416));
#5623=CARTESIAN_POINT('Ctrl Pts',(8.9532679257842,-3.7020811956009,-1.61424699855408));
#5624=CARTESIAN_POINT('Ctrl Pts',(9.01435723157795,-3.44301363458428,-0.3827306278625));
#5625=CARTESIAN_POINT('Ctrl Pts',(9.0332901097715,-3.44394015329315,-0.0006874438837658));
#5626=CARTESIAN_POINT('Ctrl Pts',(8.16670989022851,-3.44373997328344,0.000990877584210043));
#5627=CARTESIAN_POINT('Ctrl Pts',(8.18464105416476,-3.44246936070189,0.36274984291225));
#5628=CARTESIAN_POINT('Ctrl Pts',(8.2447286457012,-3.68275714716096,1.57339810621675));
#5629=CARTESIAN_POINT('Ctrl Pts',(8.34697266483782,-5.5335046738129,2.98519695992403));
#5630=CARTESIAN_POINT('Ctrl Pts',(8.47344194763839,-8.24639557638579,2.02057558976858));
#5631=CARTESIAN_POINT('Ctrl Pts',(8.59991123043898,-8.91928310048972,-0.77897683272588));
#5632=CARTESIAN_POINT('Ctrl Pts',(8.72638051323954,-6.94110269497493,-2.87112251928));
#5633=CARTESIAN_POINT('Ctrl Pts',(8.8486467331694,-4.20243074754735,-2.37305761672387));
#5634=CARTESIAN_POINT('Ctrl Pts',(8.92875652549905,-3.44196494433624,-0.759063671507021));
#5635=CARTESIAN_POINT('Ctrl Pts',(8.96670989022851,-3.43689094140915,0.00141529279526262));
#5636=CARTESIAN_POINT('Origin',(-1.7667098902285,-6.,0.));
#5637=CARTESIAN_POINT('',(7.36670989022851,-3.44040316956898,-0.00228610733910742));
#5638=CARTESIAN_POINT('',(7.4332901097715,-3.43921965943194,0.00222060329450378));
#5639=CARTESIAN_POINT('',(-1.7667098902285,-3.44,1.9679933794996E-13));
#5640=CARTESIAN_POINT('Ctrl Pts',(7.4332901097715,-3.43921965943194,0.00222060329450373));
#5641=CARTESIAN_POINT('Ctrl Pts',(7.44181343370898,-3.43766552072112,0.173408608068247));
#5642=CARTESIAN_POINT('Ctrl Pts',(7.49249318524665,-3.53110044716585,1.1896069546148));
#5643=CARTESIAN_POINT('Ctrl Pts',(7.58532936438453,-4.88860486534565,2.80959413389628));
#5644=CARTESIAN_POINT('Ctrl Pts',(7.7117986471851,-7.74719543871252,2.46502057642963));
#5645=CARTESIAN_POINT('Ctrl Pts',(7.83826792998567,-9.01911774919456,-0.118094722276079));
#5646=CARTESIAN_POINT('Ctrl Pts',(7.96473721278625,-7.54930996179144,-2.5939654930144));
#5647=CARTESIAN_POINT('Ctrl Pts',(8.09120649558682,-4.67253825597884,-2.71419668832455));
#5648=CARTESIAN_POINT('Ctrl Pts',(8.18072412791524,-3.48957571549017,-1.05464412437998));
#5649=CARTESIAN_POINT('Ctrl Pts',(8.22808533264346,-3.43656540310815,-0.106015641527535));
#5650=CARTESIAN_POINT('Ctrl Pts',(8.2332901097715,-3.43735861323486,-0.0016764958084832));
#5651=CARTESIAN_POINT('Ctrl Pts',(7.36670989022851,-3.44040316956898,-0.00228610733910735));
#5652=CARTESIAN_POINT('Ctrl Pts',(7.39836915523028,-3.44608356882379,0.634333467603688));
#5653=CARTESIAN_POINT('Ctrl Pts',(7.47218484783223,-4.00717014687453,2.12759383120187));
#5654=CARTESIAN_POINT('Ctrl Pts',(7.58815696803439,-6.50654071121665,2.97866333871112));
#5655=CARTESIAN_POINT('Ctrl Pts',(7.71462625083495,-8.77213940010801,1.20177448985872));
#5656=CARTESIAN_POINT('Ctrl Pts',(7.84109553363553,-8.52029469802955,-1.66647334565703));
#5657=CARTESIAN_POINT('Ctrl Pts',(7.96756481643611,-5.9797125579978,-3.02135850191909));
#5658=CARTESIAN_POINT('Ctrl Pts',(8.07610293530042,-3.81515252211499,-1.82939789701246));
#5659=CARTESIAN_POINT('Ctrl Pts',(8.14248462656456,-3.4454565893889,-0.487750753970042));
#5660=CARTESIAN_POINT('Ctrl Pts',(8.16670989022851,-3.44373997328344,0.000990877584210043));
#5661=CARTESIAN_POINT('Origin',(-1.7667098902285,-6.,0.));
#5662=CARTESIAN_POINT('',(6.56670989022851,-3.43650398705703,0.0011262704457668));
#5663=CARTESIAN_POINT('',(6.6332901097715,-3.44406314725449,-0.000379914237597221));
#5664=CARTESIAN_POINT('',(-1.7667098902285,-3.44,1.9679933794996E-13));
#5665=CARTESIAN_POINT('Ctrl Pts',(6.6332901097715,-3.44406314725449,-0.000379914237597229));
#5666=CARTESIAN_POINT('Ctrl Pts',(6.6555415347745,-3.44466328028651,0.448681698616593));
#5667=CARTESIAN_POINT('Ctrl Pts',(6.7199493873777,-3.77077864344925,1.749327874684));
#5668=CARTESIAN_POINT('Ctrl Pts',(6.8265136675811,-5.83926938364069,3.01714832455762));
#5669=CARTESIAN_POINT('Ctrl Pts',(6.95298295038165,-8.44009396559778,1.78184168277249));
#5670=CARTESIAN_POINT('Ctrl Pts',(7.07945223318224,-8.82501323416001,-1.07159627207705));
#5671=CARTESIAN_POINT('Ctrl Pts',(7.2059215159828,-6.6444731702528,-2.95189306651605));
#5672=CARTESIAN_POINT('Ctrl Pts',(7.3238674748459,-4.06507178369403,-2.20544952615896));
#5673=CARTESIAN_POINT('Ctrl Pts',(7.39965700610879,-3.4453523030755,-0.673288617356633));
#5674=CARTESIAN_POINT('Ctrl Pts',(7.4332901097715,-3.43921965943194,0.00222060329450373));
#5675=CARTESIAN_POINT('Ctrl Pts',(6.56670989022851,-3.43650398705703,0.00112627044576692));
#5676=CARTESIAN_POINT('Ctrl Pts',(6.56994082869561,-3.43614573843741,0.0658393894794153));
#5677=CARTESIAN_POINT('Ctrl Pts',(6.61532819476289,-3.46761353360699,0.974558132719011));
#5678=CARTESIAN_POINT('Ctrl Pts',(6.70287198843037,-4.54778863223406,2.64954730489951));
#5679=CARTESIAN_POINT('Ctrl Pts',(6.82934127123096,-7.42703945423727,2.66318928610364));
#5680=CARTESIAN_POINT('Ctrl Pts',(6.95581055403151,-9.01036300717914,0.25832797484807));
#5681=CARTESIAN_POINT('Ctrl Pts',(7.0822798368321,-7.85990684631327,-2.38112689720535));
#5682=CARTESIAN_POINT('Ctrl Pts',(7.20874911963266,-5.02042660634255,-2.85822580353484));
#5683=CARTESIAN_POINT('Ctrl Pts',(7.30355913743147,-3.55864292974095,-1.27003728223635));
#5684=CARTESIAN_POINT('Ctrl Pts',(7.35621272763009,-3.4385197375121,-0.213368051002073));
#5685=CARTESIAN_POINT('Ctrl Pts',(7.36670989022851,-3.44040316956898,-0.00228610733910735));
#5686=CARTESIAN_POINT('Origin',(-1.7667098902285,-6.,0.));
#5687=CARTESIAN_POINT('',(5.76670989022851,-3.44347757139674,0.00126671354594904));
#5688=CARTESIAN_POINT('',(5.8332901097715,-3.43786500993883,-0.00188959581389439));
#5689=CARTESIAN_POINT('',(-1.7667098902285,-3.44,1.9679933794996E-13));
#5690=CARTESIAN_POINT('Ctrl Pts',(5.8332901097715,-3.43786500993883,-0.00188959581389444));
#5691=CARTESIAN_POINT('Ctrl Pts',(5.86926963584003,-3.4438412047324,0.719757477813235));
#5692=CARTESIAN_POINT('Ctrl Pts',(5.94740558950874,-4.1378402398782,2.29700877488544));
#5693=CARTESIAN_POINT('Ctrl Pts',(6.06769797077765,-6.80660452923693,2.9117705055246));
#5694=CARTESIAN_POINT('Ctrl Pts',(6.19416725357822,-8.87991129560537,0.913854076356023));
#5695=CARTESIAN_POINT('Ctrl Pts',(6.32063653637879,-8.33790454041667,-1.91395420617355));
#5696=CARTESIAN_POINT('Ctrl Pts',(6.44710581917937,-5.67279303335752,-3.00365676208316));
#5697=CARTESIAN_POINT('Ctrl Pts',(6.55132367697694,-3.72145370847857,-1.65386257482374));
#5698=CARTESIAN_POINT('Ctrl Pts',(6.61338510717431,-3.44352629851068,-0.402087785484153));
#5699=CARTESIAN_POINT('Ctrl Pts',(6.6332901097715,-3.44406314725449,-0.000379914237597229));
#5700=CARTESIAN_POINT('Ctrl Pts',(5.76670989022851,-3.44347757139674,0.00126671354594932));
#5701=CARTESIAN_POINT('Ctrl Pts',(5.78366892976113,-3.44193188873403,0.343325238059439));
#5702=CARTESIAN_POINT('Ctrl Pts',(5.84278439689394,-3.66461387574044,1.53373597131417));
#5703=CARTESIAN_POINT('Ctrl Pts',(5.94405629162693,-5.4652566627727,2.97372970205115));
#5704=CARTESIAN_POINT('Ctrl Pts',(6.07052557442751,-8.19952879357467,2.0714950793584));
#5705=CARTESIAN_POINT('Ctrl Pts',(6.19699485722808,-8.9363583629794,-0.711911751364896));
#5706=CARTESIAN_POINT('Ctrl Pts',(6.32346414002865,-7.00661353387476,-2.84881518722965));
#5707=CARTESIAN_POINT('Ctrl Pts',(6.44670248436214,-4.2353929234673,-2.41014480803071));
#5708=CARTESIAN_POINT('Ctrl Pts',(6.52778440109542,-3.44082007134406,-0.778520212260661));
#5709=CARTESIAN_POINT('Ctrl Pts',(6.56670989022851,-3.43650398705703,0.00112627044576692));
#5710=CARTESIAN_POINT('Origin',(-1.7667098902285,-6.,0.));
#5711=CARTESIAN_POINT('',(4.96670989022851,-3.44096993331538,-0.00224703045531571));
#5712=CARTESIAN_POINT('',(5.0332901097715,-3.4386429978355,0.0021162044573253));
#5713=CARTESIAN_POINT('',(-1.7667098902285,-3.44,1.9679933794996E-13));
#5714=CARTESIAN_POINT('Ctrl Pts',(5.0332901097715,-3.4386429978355,0.00211620445732504));
#5715=CARTESIAN_POINT('Ctrl Pts',(5.04084130930535,-3.43729605427409,0.153691298419752));
#5716=CARTESIAN_POINT('Ctrl Pts',(5.0905489364394,-3.51832505384762,1.15003400307478));
#5717=CARTESIAN_POINT('Ctrl Pts',(5.18241299117364,-4.82454787213973,2.7834027086531));
#5718=CARTESIAN_POINT('Ctrl Pts',(5.3088822739742,-7.69028042141618,2.50439023325154));
#5719=CARTESIAN_POINT('Ctrl Pts',(5.43535155677479,-9.02103053977556,-0.0489164713765121));
#5720=CARTESIAN_POINT('Ctrl Pts',(5.56182083957535,-7.60831351323712,-2.55780100605334));
#5721=CARTESIAN_POINT('Ctrl Pts',(5.68829012237593,-4.73505008567186,-2.743887763315));
#5722=CARTESIAN_POINT('Ctrl Pts',(5.77877987910798,-3.50113301626044,-1.09414097539061));
#5723=CARTESIAN_POINT('Ctrl Pts',(5.82711320823984,-3.43683902736464,-0.125780691708827));
#5724=CARTESIAN_POINT('Ctrl Pts',(5.8332901097715,-3.43786500993883,-0.00188959581389444));
#5725=CARTESIAN_POINT('Ctrl Pts',(4.96670989022851,-3.44096993331538,-0.00224703045531561));
#5726=CARTESIAN_POINT('Ctrl Pts',(4.99739703082665,-3.44628149732869,0.615172962045894));
#5727=CARTESIAN_POINT('Ctrl Pts',(5.07024059902497,-3.97974614246111,2.08900564922984));
#5728=CARTESIAN_POINT('Ctrl Pts',(5.1852405948235,-6.43818709990916,2.98948337393659));
#5729=CARTESIAN_POINT('Ctrl Pts',(5.31170987762407,-8.74388782855944,1.26494994440632));
#5730=CARTESIAN_POINT('Ctrl Pts',(5.43817916042464,-8.55780106687306,-1.60831355147971));
#5731=CARTESIAN_POINT('Ctrl Pts',(5.56464844322523,-6.04891647253973,-3.02103061160996));
#5732=CARTESIAN_POINT('Ctrl Pts',(5.67415868649316,-3.83799822568673,-1.86872888720316));
#5733=CARTESIAN_POINT('Ctrl Pts',(5.74151250216093,-3.44577411453568,-0.50695672489885));
#5734=CARTESIAN_POINT('Ctrl Pts',(5.76670989022851,-3.44347757139674,0.00126671354594932));
#5735=CARTESIAN_POINT('Origin',(-1.7667098902285,-6.,0.));
#5736=CARTESIAN_POINT('',(4.16670989022851,-3.43619743813536,0.000808262677862992));
#5737=CARTESIAN_POINT('',(4.2332901097715,-3.44411439821716,-6.54012234668632E-5));
#5738=CARTESIAN_POINT('',(-1.7667098902285,-3.44,1.9679933794996E-13));
#5739=CARTESIAN_POINT('Ctrl Pts',(4.2332901097715,-3.44411439821716,-6.54012234668419E-5));
#5740=CARTESIAN_POINT('Ctrl Pts',(4.25456941037087,-3.4442130833179,0.429399038434416));
#5741=CARTESIAN_POINT('Ctrl Pts',(4.31800513857044,-3.74989810283886,1.70980757434144));
#5742=CARTESIAN_POINT('Ctrl Pts',(4.4235972943702,-5.77020937810816,3.01267565687393));
#5743=CARTESIAN_POINT('Ctrl Pts',(4.55006657717077,-8.39864413395782,1.83726009646369));
#5744=CARTESIAN_POINT('Ctrl Pts',(4.67653585997135,-8.84881511949022,-1.00661350993934));
#5745=CARTESIAN_POINT('Ctrl Pts',(4.80300514277192,-6.71191173443704,-2.93635829315832));
#5746=CARTESIAN_POINT('Ctrl Pts',(4.92192322603864,-4.09469599587263,-2.24352319467422));
#5747=CARTESIAN_POINT('Ctrl Pts',(4.99868488170516,-3.44481569780537,-0.692513923144139));
#5748=CARTESIAN_POINT('Ctrl Pts',(5.0332901097715,-3.4386429978355,0.00211620445732504));
#5749=CARTESIAN_POINT('Ctrl Pts',(4.16670989022851,-3.43619743813536,0.000808262677863087));
#5750=CARTESIAN_POINT('Ctrl Pts',(4.16896870429198,-3.43600925430327,0.0460361235042767));
#5751=CARTESIAN_POINT('Ctrl Pts',(4.21338394595564,-3.45752296120616,0.935172543509394));
#5752=CARTESIAN_POINT('Ctrl Pts',(4.29995561521949,-4.48748661387422,2.61559210015096));
#5753=CARTESIAN_POINT('Ctrl Pts',(4.42642489802005,-7.36566973169923,2.69517438424447));
#5754=CARTESIAN_POINT('Ctrl Pts',(4.55289418082063,-9.00365683350444,0.327206974422883));
#5755=CARTESIAN_POINT('Ctrl Pts',(4.67936346362121,-7.9139542516838,-2.33790459600758));
#5756=CARTESIAN_POINT('Ctrl Pts',(4.80583274642177,-5.08614590191431,-2.87991136408426));
#5757=CARTESIAN_POINT('Ctrl Pts',(4.90161488862421,-3.57301389199172,-1.30968210485211));
#5758=CARTESIAN_POINT('Ctrl Pts',(4.95524060322646,-3.43898474176898,-0.233007112912495));
#5759=CARTESIAN_POINT('Ctrl Pts',(4.96670989022851,-3.44096993331538,-0.00224703045531561));
#5760=CARTESIAN_POINT('Origin',(-1.7667098902285,-6.,0.));
#5761=CARTESIAN_POINT('',(3.36670989022851,-3.44315176552051,0.0015188218181697));
#5762=CARTESIAN_POINT('',(3.4332901097715,-3.43840959360912,-0.00205930223877143));
#5763=CARTESIAN_POINT('',(-1.7667098902285,-3.44,1.9679933794996E-13));
#5764=CARTESIAN_POINT('Ctrl Pts',(3.4332901097715,-3.43840959360912,-0.00205930223877139));
#5765=CARTESIAN_POINT('Ctrl Pts',(3.46829751143639,-3.44455735196194,0.700477811498659));
#5766=CARTESIAN_POINT('Ctrl Pts',(3.54546134070148,-4.10716776075693,2.25921769609112));
#5767=CARTESIAN_POINT('Ctrl Pts',(3.66478159756677,-6.73970426360059,2.92948049079009));
#5768=CARTESIAN_POINT('Ctrl Pts',(3.79125088036733,-8.85822573557158,0.979573370365098));
#5769=CARTESIAN_POINT('Ctrl Pts',(3.91772016316791,-8.3811268405867,-1.85990680208812));
#5770=CARTESIAN_POINT('Ctrl Pts',(4.04418944596848,-5.74167203129455,-3.01036293559842));
#5771=CARTESIAN_POINT('Ctrl Pts',(4.14937942816968,-3.74144472779083,-1.69344416525101));
#5772=CARTESIAN_POINT('Ctrl Pts',(4.21241298277068,-3.44401757824078,-0.421413067571763));
#5773=CARTESIAN_POINT('Ctrl Pts',(4.2332901097715,-3.44411439821716,-6.54012234668419E-5));
#5774=CARTESIAN_POINT('Ctrl Pts',(3.36670989022851,-3.44315176552051,0.00151882181816984));
#5775=CARTESIAN_POINT('Ctrl Pts',(3.3826968053575,-3.44139097769529,0.323866832040517));
#5776=CARTESIAN_POINT('Ctrl Pts',(3.44084014808668,-3.64706263387512,1.49406094909534));
#5777=CARTESIAN_POINT('Ctrl Pts',(3.54113991841605,-5.39728918769256,2.96070235836602));
#5778=CARTESIAN_POINT('Ctrl Pts',(3.66760920121662,-8.15150809295624,2.12132781612021));
#5779=CARTESIAN_POINT('Ctrl Pts',(3.79407848401719,-8.95189313670652,-0.644473185577155));
#5780=CARTESIAN_POINT('Ctrl Pts',(3.92054776681777,-7.07159629755764,-2.82501330133343));
#5781=CARTESIAN_POINT('Ctrl Pts',(4.04475823555487,-4.26912231760636,-2.44696890310363));
#5782=CARTESIAN_POINT('Ctrl Pts',(4.12681227669178,-3.43952134421862,-0.798055061899725));
#5783=CARTESIAN_POINT('Ctrl Pts',(4.16670989022851,-3.43619743813536,0.000808262677863087));
#5784=CARTESIAN_POINT('Origin',(-1.7667098902285,-6.,0.));
#5785=CARTESIAN_POINT('',(2.5667098902285,-3.44151252959564,-0.00216282566888451));
#5786=CARTESIAN_POINT('',(2.6332901097715,-3.43808642759416,0.00196523244380428));
#5787=CARTESIAN_POINT('',(-1.7667098902285,-3.44,1.9679933794996E-13));
#5788=CARTESIAN_POINT('Ctrl Pts',(2.6332901097715,-3.43808642759416,0.00196523244380487));
#5789=CARTESIAN_POINT('Ctrl Pts',(2.63986918490172,-3.43696448982562,0.133952481122952));
#5790=CARTESIAN_POINT('Ctrl Pts',(2.68860468763214,-3.50605985805332,1.11049088646622));
#5791=CARTESIAN_POINT('Ctrl Pts',(2.77949661796275,-4.7611075477298,2.75575104615122));
#5792=CARTESIAN_POINT('Ctrl Pts',(2.90596590076332,-7.63247864459777,2.54244603125873));
#5793=CARTESIAN_POINT('Ctrl Pts',(3.03243518356389,-9.02135843007676,0.0202874415191203));
#5794=CARTESIAN_POINT('Ctrl Pts',(3.15890446636447,-7.66647330603156,-2.52029463810126));
#5795=CARTESIAN_POINT('Ctrl Pts',(3.28537374916504,-4.79822553871722,-2.77213933419203));
#5796=CARTESIAN_POINT('Ctrl Pts',(3.37683563030072,-3.5131894475665,-1.13367101628351));
#5797=CARTESIAN_POINT('Ctrl Pts',(3.4261410838362,-3.43715413099785,-0.145527706283506));
#5798=CARTESIAN_POINT('Ctrl Pts',(3.4332901097715,-3.43840959360912,-0.00205930223877139));
#5799=CARTESIAN_POINT('Ctrl Pts',(2.5667098902285,-3.44151252959564,-0.0021628256688843));
#5800=CARTESIAN_POINT('Ctrl Pts',(2.59642490642301,-3.44638181709016,0.596020219394989));
#5801=CARTESIAN_POINT('Ctrl Pts',(2.66829635021772,-3.95303333681341,2.05027345959037));
#5802=CARTESIAN_POINT('Ctrl Pts',(2.7823242216126,-6.36960360330106,2.99873506265578));
#5803=CARTESIAN_POINT('Ctrl Pts',(2.90879350441318,-8.71419675286107,1.32746177559001));
#5804=CARTESIAN_POINT('Ctrl Pts',(3.03526278721375,-8.59396555469508,-1.5493099986334));
#5805=CARTESIAN_POINT('Ctrl Pts',(3.16173207001433,-6.1180947250836,-3.01911782098221));
#5806=CARTESIAN_POINT('Ctrl Pts',(3.27221443768591,-3.8615096110079,-1.907978510426));
#5807=CARTESIAN_POINT('Ctrl Pts',(3.34054037775731,-3.44603405760624,-0.526143344742301));
#5808=CARTESIAN_POINT('Ctrl Pts',(3.36670989022851,-3.44315176552051,0.00151882181816984));
#5809=CARTESIAN_POINT('Origin',(-1.7667098902285,-6.,0.));
#5810=CARTESIAN_POINT('',(1.76670989022851,-3.43598587725866,0.000468657341183842));
#5811=CARTESIAN_POINT('',(1.8332901097715,-3.44409311993689,0.000250277236630306));
#5812=CARTESIAN_POINT('',(-1.7667098902285,-3.44,1.9679933794996E-13));
#5813=CARTESIAN_POINT('Ctrl Pts',(1.8332901097715,-3.44409311993689,0.000250277236630361));
#5814=CARTESIAN_POINT('Ctrl Pts',(1.85359728596724,-3.44373249577201,0.410086549461726));
#5815=CARTESIAN_POINT('Ctrl Pts',(1.91606088976318,-3.72964858803878,1.67024234614915));
#5816=CARTESIAN_POINT('Ctrl Pts',(2.02068092115931,-5.70126992189332,3.00662240928013));
#5817=CARTESIAN_POINT('Ctrl Pts',(2.14715020395988,-8.35593592155457,1.89171467455323));
#5818=CARTESIAN_POINT('Ctrl Pts',(2.27361948676046,-8.87112245100439,-0.941102672625564));
#5819=CARTESIAN_POINT('Ctrl Pts',(2.40008876956103,-6.77897681420636,-2.91928303105917));
#5820=CARTESIAN_POINT('Ctrl Pts',(2.51997897723137,-4.12506033817286,-2.28139989219694));
#5821=CARTESIAN_POINT('Ctrl Pts',(2.59771275730153,-3.44415347724027,-0.711775950754531));
#5822=CARTESIAN_POINT('Ctrl Pts',(2.6332901097715,-3.43808642759416,0.00196523244380487));
#5823=CARTESIAN_POINT('Ctrl Pts',(1.76670989022851,-3.43598587725866,0.000468657341183452));
#5824=CARTESIAN_POINT('Ctrl Pts',(1.76799657988834,-3.43592048441881,0.0262261539081465));
#5825=CARTESIAN_POINT('Ctrl Pts',(1.81143969714838,-3.44790166097614,0.895826481676196));
#5826=CARTESIAN_POINT('Ctrl Pts',(1.8970392420086,-4.42797832080538,2.58026432327149));
#5827=CARTESIAN_POINT('Ctrl Pts',(2.02350852480917,-7.30358342959944,2.725745728157));
#5828=CARTESIAN_POINT('Ctrl Pts',(2.14997780760974,-8.99537493549262,0.395914211910863));
#5829=CARTESIAN_POINT('Ctrl Pts',(2.27644709041031,-7.9669975211319,-2.29345572403429));
#5830=CARTESIAN_POINT('Ctrl Pts',(2.40291637321089,-5.15234464286247,-2.90008608592962));
#5831=CARTESIAN_POINT('Ctrl Pts',(2.49967063981695,-3.58792809894497,-1.34934329362133));
#5832=CARTESIAN_POINT('Ctrl Pts',(2.55426847882282,-3.43947380248962,-0.2526167143973));
#5833=CARTESIAN_POINT('Ctrl Pts',(2.5667098902285,-3.44151252959564,-0.0021628256688843));
#5834=CARTESIAN_POINT('Origin',(-1.7667098902285,-6.,0.));
#5835=CARTESIAN_POINT('',(0.966709890228505,-3.4427709916825,0.00173622513077953));
#5836=CARTESIAN_POINT('',(1.0332901097715,-3.438979209753,-0.0021867409662462));
#5837=CARTESIAN_POINT('',(-1.7667098902285,-3.44,1.9679933794996E-13));
#5838=CARTESIAN_POINT('Ctrl Pts',(1.0332901097715,-3.438979209753,-0.00218674096624601));
#5839=CARTESIAN_POINT('Ctrl Pts',(1.06732538703276,-3.44514488069256,0.681234816892835));
#5840=CARTESIAN_POINT('Ctrl Pts',(1.14351709189422,-4.07723850978797,2.22122910905365));
#5841=CARTESIAN_POINT('Ctrl Pts',(1.26186522435587,-6.67241573405984,2.94565054354541));
#5842=CARTESIAN_POINT('Ctrl Pts',(1.38833450715645,-8.83504078941567,1.04478035722949));
#5843=CARTESIAN_POINT('Ctrl Pts',(1.51480378995702,-8.42309989372086,-1.8048844843804));
#5844=CARTESIAN_POINT('Ctrl Pts',(1.64127307275759,-5.81068658220031,-3.01548936826444));
#5845=CARTESIAN_POINT('Ctrl Pts',(1.74743517936242,-3.76206314555082,-1.73298420137006));
#5846=CARTESIAN_POINT('Ctrl Pts',(1.81144085836705,-3.44448112898182,-0.440707917058323));
#5847=CARTESIAN_POINT('Ctrl Pts',(1.8332901097715,-3.44409311993689,0.000250277236630361));
#5848=CARTESIAN_POINT('Ctrl Pts',(0.966709890228505,-3.4427709916825,0.00173622513077922));
#5849=CARTESIAN_POINT('Ctrl Pts',(0.981724680953865,-3.44085207515589,0.304374748864834));
#5850=CARTESIAN_POINT('Ctrl Pts',(1.03889589927942,-3.63008029168738,1.45440282564708));
#5851=CARTESIAN_POINT('Ctrl Pts',(1.13822354520516,-5.32964905792872,2.94610338914275));
#5852=CARTESIAN_POINT('Ctrl Pts',(1.26469282800573,-8.10235283801081,2.17005725520049));
#5853=CARTESIAN_POINT('Ctrl Pts',(1.3911621108063,-8.96588232345381,-0.576701529052951));
#5854=CARTESIAN_POINT('Ctrl Pts',(1.51763139360688,-7.13601528805713,-2.7997267301126));
#5855=CARTESIAN_POINT('Ctrl Pts',(1.64281398674761,-4.30362504627695,-2.48351527668098));
#5856=CARTESIAN_POINT('Ctrl Pts',(1.72584015228815,-3.43806298124983,-0.817679002928948));
#5857=CARTESIAN_POINT('Ctrl Pts',(1.76670989022851,-3.43598587725866,0.000468657341183452));
#5858=CARTESIAN_POINT('Origin',(-1.7667098902285,-6.,0.));
#5859=CARTESIAN_POINT('',(0.166709890228505,-3.44261795854501,-0.003041210415346));
#5860=CARTESIAN_POINT('',(0.233290109771496,-3.4375580541705,0.00169662369046232));
#5861=CARTESIAN_POINT('',(-1.7667098902285,-3.44,1.9679933794996E-13));
#5862=CARTESIAN_POINT('',(0.,-5.33826273143149,-2.47299490241842));
#5863=CARTESIAN_POINT('Ctrl Pts',(0.,-5.33826273143149,-2.47299490241842));
#5864=CARTESIAN_POINT('Ctrl Pts',(0.042156427600191,-4.51946448572409,-2.25389646671472));
#5865=CARTESIAN_POINT('Ctrl Pts',(0.0977263910096926,-3.60391090134556,
-1.38973602151771));
#5866=CARTESIAN_POINT('Ctrl Pts',(0.153296354419194,-3.44063791734118,-0.273280262488538));
#5867=CARTESIAN_POINT('Ctrl Pts',(0.166709890228505,-3.44261795854501,-0.00304121041534603));
#5868=CARTESIAN_POINT('',(1.04028532515104E-16,-6.66309219466394,-2.47735541001815));
#5869=CARTESIAN_POINT('Origin',(0.,-6.,0.));
#5870=CARTESIAN_POINT('Ctrl Pts',(-4.13352078260099E-17,-6.66309273064559,
-2.4773571349477));
#5871=CARTESIAN_POINT('Ctrl Pts',(0.0412138930502382,-5.86569025594692,
-2.68954112476757));
#5872=CARTESIAN_POINT('Ctrl Pts',(0.11897726297407,-4.14769481245353,-2.29913676584276));
#5873=CARTESIAN_POINT('Ctrl Pts',(0.196740632897902,-3.44336669350132,-0.730968858270161));
#5874=CARTESIAN_POINT('Ctrl Pts',(0.233290109771496,-3.4375580541705,0.00169662369046196));
#5875=CARTESIAN_POINT('Origin',(6.,6.,0.));
#5876=CARTESIAN_POINT('',(10.0890562790225,8.11715687076559,0.00188038179815303));
#5877=CARTESIAN_POINT('',(10.3109437209775,8.11380015351683,0.000572561662963434));
#5878=CARTESIAN_POINT('',(6.,8.117,2.59257727379495E-16));
#5879=CARTESIAN_POINT('',(11.,7.36291222925732,-1.61992569438875));
#5880=CARTESIAN_POINT('Ctrl Pts',(10.3109437209775,8.11380015351683,0.000572561662963434));
#5881=CARTESIAN_POINT('Ctrl Pts',(10.3298470093174,8.11459727114496,0.316007738993721));
#5882=CARTESIAN_POINT('Ctrl Pts',(10.3487502976573,8.04842739124356,0.631134507362876));
#5883=CARTESIAN_POINT('Ctrl Pts',(10.3676535859971,7.91360200006723,0.913504858331154));
#5884=CARTESIAN_POINT('Ctrl Pts',(10.4098100135973,7.61292643824968,1.54322202938665));
#5885=CARTESIAN_POINT('Ctrl Pts',(10.4519664411975,6.97079995430339,2.01002862386259));
#5886=CARTESIAN_POINT('Ctrl Pts',(10.4941228687977,6.27919611550385,2.10193932389814));
#5887=CARTESIAN_POINT('Ctrl Pts',(10.5362792963979,5.58759227670429,2.19385002393369));
#5888=CARTESIAN_POINT('Ctrl Pts',(10.5784357239981,4.84651108305146,1.91086482952882));
#5889=CARTESIAN_POINT('Ctrl Pts',(10.6205921515983,4.39166122021261,1.38152854464845));
#5890=CARTESIAN_POINT('Ctrl Pts',(10.6627485791985,3.93681135737378,0.852192259768091));
#5891=CARTESIAN_POINT('Ctrl Pts',(10.7049050067987,3.7681928253489,0.07650488441227));
#5892=CARTESIAN_POINT('Ctrl Pts',(10.7470614343988,3.96392499548221,-0.593437324111172));
#5893=CARTESIAN_POINT('Ctrl Pts',(10.789217861999,4.15965716561551,-1.26337953263462));
#5894=CARTESIAN_POINT('Ctrl Pts',(10.8313742895992,4.71974003790703,-1.82757657432568));
#5895=CARTESIAN_POINT('Ctrl Pts',(10.8735307171994,5.38646615209559,-2.02952674625186));
#5896=CARTESIAN_POINT('Ctrl Pts',(10.9156871447996,6.05319226628417,-2.23147691817804));
#5897=CARTESIAN_POINT('Ctrl Pts',(10.9578435723998,6.8265616223698,-2.07118022033934));
#5898=CARTESIAN_POINT('Ctrl Pts',(11.,7.36291222925732,-1.61992569438875));
#5899=CARTESIAN_POINT('',(11.,7.36522651177467,1.62290944688048));
#5900=CARTESIAN_POINT('Origin',(11.,6.,0.));
#5901=CARTESIAN_POINT('',(10.8890562790225,8.11943734836568,-0.00125295574427895));
#5902=CARTESIAN_POINT('Ctrl Pts',(11.,7.36522742428751,1.6229106233628));
#5903=CARTESIAN_POINT('Ctrl Pts',(10.9630187596742,7.83319589372452,1.22807491081379));
#5904=CARTESIAN_POINT('Ctrl Pts',(10.9260375193483,8.11557054190741,0.611672144507363));
#5905=CARTESIAN_POINT('Ctrl Pts',(10.8890562790225,8.11943734836568,-0.00125295574427895));
#5906=CARTESIAN_POINT('',(12.,8.117,-2.59257727379495E-16));
#5907=CARTESIAN_POINT('',(6.,8.117,2.59257727379495E-16));
#5908=CARTESIAN_POINT('Origin',(12.,6.,0.));
#5909=CARTESIAN_POINT('Ctrl Pts',(10.8890562790225,8.11943734836568,-0.00125295574427895));
#5910=CARTESIAN_POINT('Ctrl Pts',(10.8848236262981,8.11987992002488,-0.071404715733393));
#5911=CARTESIAN_POINT('Ctrl Pts',(10.8805909735737,8.11667411428522,-0.14151091923779));
#5912=CARTESIAN_POINT('Ctrl Pts',(10.8763583208493,8.10968062356725,-0.211234152861468));
#5913=CARTESIAN_POINT('Ctrl Pts',(10.8342018932491,8.04002676715129,-0.905664488088106));
#5914=CARTESIAN_POINT('Ctrl Pts',(10.7920454656489,7.59464264590244,-1.56210502861697));
#5915=CARTESIAN_POINT('Ctrl Pts',(10.7498890380487,6.97508320827158,-1.88289980549192));
#5916=CARTESIAN_POINT('Ctrl Pts',(10.7077326104485,6.35552377064071,-2.20369458236686));
#5917=CARTESIAN_POINT('Ctrl Pts',(10.6655761828483,5.56178901662783,-2.18884359558788));
#5918=CARTESIAN_POINT('Ctrl Pts',(10.6234197552481,4.95463419811742,-1.84487767155484));
#5919=CARTESIAN_POINT('Ctrl Pts',(10.5812633276479,4.34747937960703,-1.50091174752182));
#5920=CARTESIAN_POINT('Ctrl Pts',(10.5391069000478,3.9269044965991,-0.827830886234752));
#5921=CARTESIAN_POINT('Ctrl Pts',(10.4969504724476,3.88369336722059,-0.131366067674812));
#5922=CARTESIAN_POINT('Ctrl Pts',(10.4547940448474,3.84048223784208,0.565098750885158));
#5923=CARTESIAN_POINT('Ctrl Pts',(10.4126376172472,4.17463486209302,1.28494752671801));
#5924=CARTESIAN_POINT('Ctrl Pts',(10.370481189647,4.73452101011657,1.70138259696357));
#5925=CARTESIAN_POINT('Ctrl Pts',(10.3283247620468,5.2944071581401,2.11781766720914));
#5926=CARTESIAN_POINT('Ctrl Pts',(10.2861683344466,6.08002682993622,2.23083903186743));
#5927=CARTESIAN_POINT('Ctrl Pts',(10.2440119068464,6.7346104515374,1.98909777508149));
#5928=CARTESIAN_POINT('Ctrl Pts',(10.2018554792462,7.38919407313857,1.74735651829556));
#5929=CARTESIAN_POINT('Ctrl Pts',(10.159699051646,7.9127416445448,1.15085264006539));
#5930=CARTESIAN_POINT('Ctrl Pts',(10.1175426240458,8.06755648403457,0.470451384772961));
#5931=CARTESIAN_POINT('Ctrl Pts',(10.1080471757047,8.10242747274249,0.317195633784494));
#5932=CARTESIAN_POINT('Ctrl Pts',(10.0985517273636,8.11859099220767,0.159683391670918));
#5933=CARTESIAN_POINT('Ctrl Pts',(10.0890562790225,8.11715687076559,0.00188038179815303));
#5934=CARTESIAN_POINT('Origin',(6.,6.,0.));
#5935=CARTESIAN_POINT('',(9.28905627902251,8.11374159717219,-0.000568483884271914));
#5936=CARTESIAN_POINT('',(9.5109437209775,8.11714715018758,-0.00188412167347644));
#5937=CARTESIAN_POINT('',(6.,8.117,2.59257727379495E-16));
#5938=CARTESIAN_POINT('Ctrl Pts',(9.5109437209775,8.11714715018758,-0.00188412167347644));
#5939=CARTESIAN_POINT('Ctrl Pts',(9.5435751103829,8.11222033535175,0.540420570882553));
#5940=CARTESIAN_POINT('Ctrl Pts',(9.5762064997883,7.89950915526723,1.08616073405186));
#5941=CARTESIAN_POINT('Ctrl Pts',(9.6088378891937,7.5239486527264,1.47435339986777));
#5942=CARTESIAN_POINT('Ctrl Pts',(9.65099431679389,7.03876278037019,1.97585873903933));
#5943=CARTESIAN_POINT('Ctrl Pts',(9.69315074439408,6.28178130531125,2.21441722432417));
#5944=CARTESIAN_POINT('Ctrl Pts',(9.73530717199427,5.59672863575656,2.08170810641676));
#5945=CARTESIAN_POINT('Ctrl Pts',(9.77746359959447,4.91167596620186,1.94899898850936));
#5946=CARTESIAN_POINT('Ctrl Pts',(9.81962002719466,4.29855210215141,1.44502226740969));
#5947=CARTESIAN_POINT('Ctrl Pts',(9.86177645479485,4.03573710510172,0.798615374023543));
#5948=CARTESIAN_POINT('Ctrl Pts',(9.90393288239503,3.77292210805203,0.152208480637401));
#5949=CARTESIAN_POINT('Ctrl Pts',(9.94608930999522,3.86041597800307,-0.636628585035204));
#5950=CARTESIAN_POINT('Ctrl Pts',(9.98824573759542,4.25852148728445,-1.20971725556392));
#5951=CARTESIAN_POINT('Ctrl Pts',(10.0304021651956,4.65662699656582,-1.78280592609263));
#5952=CARTESIAN_POINT('Ctrl Pts',(10.0725585927958,5.36534414517754,-2.14014620147742));
#5953=CARTESIAN_POINT('Ctrl Pts',(10.114715020396,6.06281364406225,-2.11947989435853));
#5954=CARTESIAN_POINT('Ctrl Pts',(10.1568714479962,6.76028314294696,-2.09881358723964));
#5955=CARTESIAN_POINT('Ctrl Pts',(10.1990278755964,7.44650499210468,-1.70014069761706));
#5956=CARTESIAN_POINT('Ctrl Pts',(10.2411843031966,7.81000359683914,-1.10449037898824));
#5957=CARTESIAN_POINT('Ctrl Pts',(10.2644374424569,8.0105064420276,-0.775934554930158));
#5958=CARTESIAN_POINT('Ctrl Pts',(10.2876905817172,8.11281961050863,-0.387447658639123));
#5959=CARTESIAN_POINT('Ctrl Pts',(10.3109437209775,8.11380015351683,0.000572561662963434));
#5960=CARTESIAN_POINT('Ctrl Pts',(10.0890562790225,8.11715687076559,0.00188038179815303));
#5961=CARTESIAN_POINT('Ctrl Pts',(10.0563952997634,8.11222400093238,-0.540906082550074));
#5962=CARTESIAN_POINT('Ctrl Pts',(10.0237343205044,7.8990905658408,-1.08713266777252));
#5963=CARTESIAN_POINT('Ctrl Pts',(9.99107334124528,7.5229210427651,-1.4754142144647));
#5964=CARTESIAN_POINT('Ctrl Pts',(9.94891691364509,7.03738865443255,-1.97657992605523));
#5965=CARTESIAN_POINT('Ctrl Pts',(9.90676048604489,6.28024177019415,-2.21461271688159));
#5966=CARTESIAN_POINT('Ctrl Pts',(9.8646040584447,5.59527874399254,-2.08142674968445));
#5967=CARTESIAN_POINT('Ctrl Pts',(9.82244763084451,4.91031571779093,-1.9482407824873));
#5968=CARTESIAN_POINT('Ctrl Pts',(9.78029120324432,4.29753654962611,-1.44383605726662));
#5969=CARTESIAN_POINT('Ctrl Pts',(9.73813477564413,4.03517692714596,-0.797245582009668));
#5970=CARTESIAN_POINT('Ctrl Pts',(9.69597834804394,3.77281730466582,-0.150655106752722));
#5971=CARTESIAN_POINT('Ctrl Pts',(9.65382192044375,3.86087722787033,0.638121118540479));
#5972=CARTESIAN_POINT('Ctrl Pts',(9.61166549284355,4.25937402385499,1.21093137919616));
#5973=CARTESIAN_POINT('Ctrl Pts',(9.56950906524336,4.65787081983965,1.78374163985182));
#5974=CARTESIAN_POINT('Ctrl Pts',(9.52735263764317,5.36680448860446,2.14058593586996));
#5975=CARTESIAN_POINT('Ctrl Pts',(9.48519621004299,6.06427454878569,2.11943440510194));
#5976=CARTESIAN_POINT('Ctrl Pts',(9.44303978244279,6.76174460896693,2.09828287433392));
#5977=CARTESIAN_POINT('Ctrl Pts',(9.4008833548426,7.44775106056461,1.69913551677972));
#5978=CARTESIAN_POINT('Ctrl Pts',(9.35872692724241,7.81080533581827,1.10323009083302));
#5979=CARTESIAN_POINT('Ctrl Pts',(9.33550337783578,8.01080826250376,0.774951821326824));
#5980=CARTESIAN_POINT('Ctrl Pts',(9.31227982842914,8.11280177200639,0.386961479812062));
#5981=CARTESIAN_POINT('Ctrl Pts',(9.28905627902251,8.11374159717219,-0.000568483884271914));
#5982=CARTESIAN_POINT('Origin',(6.,6.,0.));
#5983=CARTESIAN_POINT('',(8.4890562790225,8.1191842221883,-0.0013863833942596));
#5984=CARTESIAN_POINT('',(8.7109437209775,8.11957111380812,0.00117038083020428));
#5985=CARTESIAN_POINT('',(6.,8.117,2.59257727379495E-16));
#5986=CARTESIAN_POINT('Ctrl Pts',(8.7109437209775,8.11957111380812,0.00117038083020428));
#5987=CARTESIAN_POINT('Ctrl Pts',(8.71514678384822,8.12003578657627,0.0708143820557132));
#5988=CARTESIAN_POINT('Ctrl Pts',(8.71934984671895,8.11689802002172,0.140416012359908));
#5989=CARTESIAN_POINT('Ctrl Pts',(8.72355290958968,8.1100195150437,0.209645972704743));
#5990=CARTESIAN_POINT('Ctrl Pts',(8.76570933718987,8.04102858961091,0.904017648980825));
#5991=CARTESIAN_POINT('Ctrl Pts',(8.80786576479007,7.59572124303596,1.56099951257333));
#5992=CARTESIAN_POINT('Ctrl Pts',(8.85002219239026,6.9762942964785,1.88228141737542));
#5993=CARTESIAN_POINT('Ctrl Pts',(8.89217861999045,6.35686734992103,2.2035633221775));
#5994=CARTESIAN_POINT('Ctrl Pts',(8.93433504759064,5.56332080338105,2.18914526818917));
#5995=CARTESIAN_POINT('Ctrl Pts',(8.97649147519083,4.95597373781604,1.84557392740617));
#5996=CARTESIAN_POINT('Ctrl Pts',(9.01864790279102,4.34862667225104,1.50200258662317));
#5997=CARTESIAN_POINT('Ctrl Pts',(9.06080433039121,3.92747908766101,0.829277959045507));
#5998=CARTESIAN_POINT('Ctrl Pts',(9.1029607579914,3.88375755383572,0.132858399714689));
#5999=CARTESIAN_POINT('Ctrl Pts',(9.14511718559159,3.84003602001042,-0.563561159616129));
#6000=CARTESIAN_POINT('Ctrl Pts',(9.18727361319178,4.17374053694986,-1.2836756507001));
#6001=CARTESIAN_POINT('Ctrl Pts',(9.22943004079197,4.73334935747058,-1.70050886767758));
#6002=CARTESIAN_POINT('Ctrl Pts',(9.27158646839217,5.2929581779913,-2.11734208465505));
#6003=CARTESIAN_POINT('Ctrl Pts',(9.31374289599236,6.07847130209331,-2.23089402752604));
#6004=CARTESIAN_POINT('Ctrl Pts',(9.35589932359255,6.73321630384336,-1.98960505813209));
#6005=CARTESIAN_POINT('Ctrl Pts',(9.39805575119274,7.3879613055934,-1.74831608873814));
#6006=CARTESIAN_POINT('Ctrl Pts',(9.44021217879293,7.9119381849915,-1.15218620707927));
#6007=CARTESIAN_POINT('Ctrl Pts',(9.48236860639312,8.06723148986381,-0.471895169720698));
#6008=CARTESIAN_POINT('Ctrl Pts',(9.49189364458791,8.10231925096,-0.318186744142753));
#6009=CARTESIAN_POINT('Ctrl Pts',(9.50141868278271,8.11858527771892,-0.160181791614469));
#6010=CARTESIAN_POINT('Ctrl Pts',(9.5109437209775,8.11714715018758,-0.00188412167347644));
#6011=CARTESIAN_POINT('Ctrl Pts',(9.28905627902251,8.11374159717219,-0.000568483884271914));
#6012=CARTESIAN_POINT('Ctrl Pts',(9.27012340082895,8.11450778476374,-0.316500276675629));
#6013=CARTESIAN_POINT('Ctrl Pts',(9.25119052263539,8.04811125783102,-0.632126091271384));
#6014=CARTESIAN_POINT('Ctrl Pts',(9.23225764444183,7.91290253697904,-0.914842607688629));
#6015=CARTESIAN_POINT('Ctrl Pts',(9.19010121684164,7.61184336397646,-1.54434638592439));
#6016=CARTESIAN_POINT('Ctrl Pts',(9.14794478924145,6.96962291906164,-2.01069044805671));
#6017=CARTESIAN_POINT('Ctrl Pts',(9.10578836164126,6.27784890751461,-2.10212583511627));
#6018=CARTESIAN_POINT('Ctrl Pts',(9.06363193404107,5.58607489596759,-2.19356122217583));
#6019=CARTESIAN_POINT('Ctrl Pts',(9.02147550644089,4.84474731778836,-1.91008793416263));
#6020=CARTESIAN_POINT('Ctrl Pts',(8.9793190788407,4.3904743882459,-1.38042031528924));
#6021=CARTESIAN_POINT('Ctrl Pts',(8.9371626512405,3.93620145870344,-0.850752696415834));
#6022=CARTESIAN_POINT('Ctrl Pts',(8.89500622364031,3.76898317779776,-0.0748907466822245));
#6023=CARTESIAN_POINT('Ctrl Pts',(8.85284979604011,3.96474696381566,0.594876539297566));
#6024=CARTESIAN_POINT('Ctrl Pts',(8.81069336843992,4.16051074983357,1.26464382527735));
#6025=CARTESIAN_POINT('Ctrl Pts',(8.76853694083973,4.71925660277507,1.82831644750333));
#6026=CARTESIAN_POINT('Ctrl Pts',(8.72638051323954,5.38727953775154,2.02995237312644));
#6027=CARTESIAN_POINT('Ctrl Pts',(8.68422408563935,6.05530247272803,2.23158829874956));
#6028=CARTESIAN_POINT('Ctrl Pts',(8.64206765803917,6.83260248973948,2.07118752776983));
#6029=CARTESIAN_POINT('Ctrl Pts',(8.59991123043898,7.36623761004502,1.62158187684418));
#6030=CARTESIAN_POINT('Ctrl Pts',(8.56295957996682,7.83398830828272,1.22748608151556));
#6031=CARTESIAN_POINT('Ctrl Pts',(8.52600792949466,8.11452728017455,0.611189445711882));
#6032=CARTESIAN_POINT('Ctrl Pts',(8.4890562790225,8.1191842221883,-0.0013863833942596));
#6033=CARTESIAN_POINT('Origin',(6.,6.,0.));
#6034=CARTESIAN_POINT('',(7.6890562790225,8.11764522427697,0.00183633476372319));
#6035=CARTESIAN_POINT('',(7.9109437209775,8.11390728528231,0.000819409340793068));
#6036=CARTESIAN_POINT('',(6.,8.117,2.59257727379495E-16));
#6037=CARTESIAN_POINT('Ctrl Pts',(7.9109437209775,8.11390728528231,0.000819409340793068));
#6038=CARTESIAN_POINT('Ctrl Pts',(7.92887488491374,8.11495802236128,0.299977125821297));
#6039=CARTESIAN_POINT('Ctrl Pts',(7.94680604884999,8.0556605354732,0.598737210873491));
#6040=CARTESIAN_POINT('Ctrl Pts',(7.96473721278624,7.93396030919504,0.869443135120387));
#6041=CARTESIAN_POINT('Ctrl Pts',(8.00689364038643,7.64784130452458,1.50587670613843));
#6042=CARTESIAN_POINT('Ctrl Pts',(8.04905006798663,7.01680554234725,1.98724737007717));
#6043=CARTESIAN_POINT('Ctrl Pts',(8.09120649558682,6.32738204764409,2.09498325502854));
#6044=CARTESIAN_POINT('Ctrl Pts',(8.13336292318701,5.63795855294095,2.20271913997992));
#6045=CARTESIAN_POINT('Ctrl Pts',(8.1755193507872,4.89014732571198,1.93682024594394));
#6046=CARTESIAN_POINT('Ctrl Pts',(8.21767577838739,4.42350063564333,1.41802101580699));
#6047=CARTESIAN_POINT('Ctrl Pts',(8.25983220598758,3.95685394557466,0.899221785670026));
#6048=CARTESIAN_POINT('Ctrl Pts',(8.30198863358777,3.77137179266632,0.127522219432072));
#6049=CARTESIAN_POINT('Ctrl Pts',(8.34414506118796,3.95127446966703,-0.546678641855785));
#6050=CARTESIAN_POINT('Ctrl Pts',(8.38630148878815,4.13117714666773,-1.22087950314363));
#6051=CARTESIAN_POINT('Ctrl Pts',(8.42845791638834,4.67646465357747,-1.79758165948139));
#6052=CARTESIAN_POINT('Ctrl Pts',(8.47061434398854,5.33954295512743,-2.01492688192885));
#6053=CARTESIAN_POINT('Ctrl Pts',(8.51277077158873,6.00262125667738,-2.2322721043763));
#6054=CARTESIAN_POINT('Ctrl Pts',(8.55492719918893,6.78349035286756,-2.09026039293348));
#6055=CARTESIAN_POINT('Ctrl Pts',(8.59708362678912,7.32758764881733,-1.65337379273224));
#6056=CARTESIAN_POINT('Ctrl Pts',(8.63503699151858,7.81743757911368,-1.26004548132718));
#6057=CARTESIAN_POINT('Ctrl Pts',(8.67299035624804,8.11537515110373,-0.627710095390964));
#6058=CARTESIAN_POINT('Ctrl Pts',(8.7109437209775,8.11957111380812,0.00117038083020428));
#6059=CARTESIAN_POINT('Ctrl Pts',(8.4890562790225,8.1191842221883,-0.0013863833942596));
#6060=CARTESIAN_POINT('Ctrl Pts',(8.48385150189447,8.11984016975681,-0.0876699627142483));
#6061=CARTESIAN_POINT('Ctrl Pts',(8.47864672476643,8.11502268181792,-0.173879722092055));
#6062=CARTESIAN_POINT('Ctrl Pts',(8.4734419476384,8.10448396876637,-0.259384322358413));
#6063=CARTESIAN_POINT('Ctrl Pts',(8.4312855200382,8.01912498358259,-0.95193433976384));
#6064=CARTESIAN_POINT('Ctrl Pts',(8.38912909243802,7.55843678961539,-1.59822384370313));
#6065=CARTESIAN_POINT('Ctrl Pts',(8.34697266483783,6.9316001490884,-1.90479766919029));
#6066=CARTESIAN_POINT('Ctrl Pts',(8.30481623723763,6.30476350856141,-2.21137149467746));
#6067=CARTESIAN_POINT('Ctrl Pts',(8.26265980963744,5.51177842147463,-2.17822964171251));
#6068=CARTESIAN_POINT('Ctrl Pts',(8.22050338203725,4.91270886183563,-1.82042054975661));
#6069=CARTESIAN_POINT('Ctrl Pts',(8.17834695443706,4.31363930219663,-1.46261145780071));
#6070=CARTESIAN_POINT('Ctrl Pts',(8.13619052683687,3.90848527000542,-0.780135126853865));
#6071=CARTESIAN_POINT('Ctrl Pts',(8.09403409923668,3.88121160212363,-0.0828777635467605));
#6072=CARTESIAN_POINT('Ctrl Pts',(8.05187767163649,3.85393793424184,0.614379599760344));
#6073=CARTESIAN_POINT('Ctrl Pts',(8.00972124403629,4.20454463066947,1.32641799542771));
#6074=CARTESIAN_POINT('Ctrl Pts',(7.9675648164361,4.77383469847484,1.72992822147259));
#6075=CARTESIAN_POINT('Ctrl Pts',(7.92540838883591,5.3431247662802,2.13343844751747));
#6076=CARTESIAN_POINT('Ctrl Pts',(7.88325196123572,6.13109820546331,2.22842050393988));
#6077=CARTESIAN_POINT('Ctrl Pts',(7.84109553363553,6.77996663691654,1.97174669856434));
#6078=CARTESIAN_POINT('Ctrl Pts',(7.79893910603534,7.42883506836976,1.71507289318879));
#6079=CARTESIAN_POINT('Ctrl Pts',(7.75678267843515,7.93859849209309,1.1067432260153));
#6080=CARTESIAN_POINT('Ctrl Pts',(7.71462625083496,8.07779297766,0.422976760830654));
#6081=CARTESIAN_POINT('Ctrl Pts',(7.70610292689747,8.10593577244447,0.284730628221179));
#6082=CARTESIAN_POINT('Ctrl Pts',(7.69757960295999,8.11893042409154,0.143400784872793));
#6083=CARTESIAN_POINT('Ctrl Pts',(7.6890562790225,8.11764522427697,0.00183633476372319));
#6084=CARTESIAN_POINT('Origin',(6.,6.,0.));
#6085=CARTESIAN_POINT('',(6.8890562790225,8.11363988703895,-0.00031417125408606));
#6086=CARTESIAN_POINT('',(7.1109437209775,8.11666666562943,-0.00189050366901346));
#6087=CARTESIAN_POINT('',(6.,8.117,2.59257727379495E-16));
#6088=CARTESIAN_POINT('Ctrl Pts',(7.1109437209775,8.11666666562943,-0.00189050366901346));
#6089=CARTESIAN_POINT('Ctrl Pts',(7.14260298597926,8.11196924156364,0.52456406017017));
#6090=CARTESIAN_POINT('Ctrl Pts',(7.17426225098103,7.91296473303274,1.05418917756107));
#6091=CARTESIAN_POINT('Ctrl Pts',(7.2059215159828,7.55731496712391,1.43906356250341));
#6092=CARTESIAN_POINT('Ctrl Pts',(7.248077943583,7.08374353055638,1.9515495328215));
#6093=CARTESIAN_POINT('Ctrl Pts',(7.29023437118319,6.33242904651292,2.2073822840917));
#6094=CARTESIAN_POINT('Ctrl Pts',(7.33239079878338,5.64451447516916,2.09039802080721));
#6095=CARTESIAN_POINT('Ctrl Pts',(7.37454722638357,4.9565999038254,1.97341375752272));
#6096=CARTESIAN_POINT('Ctrl Pts',(7.41670365398376,4.33208524518135,1.48361247968354));
#6097=CARTESIAN_POINT('Ctrl Pts',(7.45886008158395,4.05453854420681,0.843394076261605));
#6098=CARTESIAN_POINT('Ctrl Pts',(7.50101650918415,3.77699184323228,0.203175672839669));
#6099=CARTESIAN_POINT('Ctrl Pts',(7.54317293678434,3.84641309992727,-0.58745985616502));
#6100=CARTESIAN_POINT('Ctrl Pts',(7.58532936438453,4.23128079618797,-1.16951537899457));
#6101=CARTESIAN_POINT('Ctrl Pts',(7.62748579198472,4.61614849244866,-1.75157090182411));
#6102=CARTESIAN_POINT('Ctrl Pts',(7.6696422195849,5.31646262827508,-2.12504641847851));
#6103=CARTESIAN_POINT('Ctrl Pts',(7.7117986471851,6.01423753687015,-2.12036108629895));
#6104=CARTESIAN_POINT('Ctrl Pts',(7.75395507478529,6.71201244546522,-2.1156757541194));
#6105=CARTESIAN_POINT('Ctrl Pts',(7.79611150238549,7.40724812682894,-1.73282957310589));
#6106=CARTESIAN_POINT('Ctrl Pts',(7.83826792998568,7.78426484392901,-1.14565824355045));
#6107=CARTESIAN_POINT('Ctrl Pts',(7.86249319364962,8.0009181491873,-0.808239228607084));
#6108=CARTESIAN_POINT('Ctrl Pts',(7.88671845731356,8.11248772418353,-0.403347023167936));
#6109=CARTESIAN_POINT('Ctrl Pts',(7.9109437209775,8.11390728528231,0.000819409340793068));
#6110=CARTESIAN_POINT('Ctrl Pts',(7.6890562790225,8.11764522427697,0.00183633476372319));
#6111=CARTESIAN_POINT('Ctrl Pts',(7.6554231753598,8.11257381564489,-0.55677810490725));
#6112=CARTESIAN_POINT('Ctrl Pts',(7.62179007169709,7.88515114816674,-1.11904560138433));
#6113=CARTESIAN_POINT('Ctrl Pts',(7.58815696803438,7.4887278443704,-1.5099080778379));
#6114=CARTESIAN_POINT('Ctrl Pts',(7.54600054043419,6.99184267810341,-1.99982318812603));
#6115=CARTESIAN_POINT('Ctrl Pts',(7.503844112834,6.22944679815893,-2.22045014550648));
#6116=CARTESIAN_POINT('Ctrl Pts',(7.46168768523381,5.54771479964697,-2.07161074906936));
#6117=CARTESIAN_POINT('Ctrl Pts',(7.41953125763362,4.86598280113501,-1.92277135263224));
#6118=CARTESIAN_POINT('Ctrl Pts',(7.37737483003343,4.26491468405557,-1.40446560237755));
#6119=CARTESIAN_POINT('Ctrl Pts',(7.33521840243324,4.01743232216016,-0.752036169962131));
#6120=CARTESIAN_POINT('Ctrl Pts',(7.29306197483305,3.76994996026475,-0.0996067375467069));
#6121=CARTESIAN_POINT('Ctrl Pts',(7.25090554723286,3.87605335355337,0.686946377029455));
#6122=CARTESIAN_POINT('Ctrl Pts',(7.20874911963266,4.28756503912573,1.25047970911464));
#6123=CARTESIAN_POINT('Ctrl Pts',(7.16659269203248,4.6990767246981,1.81401304119983));
#6124=CARTESIAN_POINT('Ctrl Pts',(7.12443626443228,5.41599670255422,2.15452659079405));
#6125=CARTESIAN_POINT('Ctrl Pts',(7.08227983683209,6.11279923257889,2.11740627449295));
#6126=CARTESIAN_POINT('Ctrl Pts',(7.0401234092319,6.80960176260356,2.08028595819184));
#6127=CARTESIAN_POINT('Ctrl Pts',(6.99796698163171,7.4862868447968,1.66553177599542));
#6128=CARTESIAN_POINT('Ctrl Pts',(6.95581055403152,7.8355978549684,1.06146762219652));
#6129=CARTESIAN_POINT('Ctrl Pts',(6.93355912902851,8.01997466742683,0.74262447109424));
#6130=CARTESIAN_POINT('Ctrl Pts',(6.91130770402551,8.11314360517165,0.371038718645036));
#6131=CARTESIAN_POINT('Ctrl Pts',(6.8890562790225,8.11363988703895,-0.00031417125408606));
#6132=CARTESIAN_POINT('Origin',(6.,6.,0.));
#6133=CARTESIAN_POINT('',(6.0890562790225,8.11876545586576,-0.0015626071037439));
#6134=CARTESIAN_POINT('',(6.3109437209775,8.11989110689617,0.00093137289447728));
#6135=CARTESIAN_POINT('',(6.,8.117,2.59257727379495E-16));
#6136=CARTESIAN_POINT('Ctrl Pts',(6.3109437209775,8.11989110689617,0.00093137289447728));
#6137=CARTESIAN_POINT('Ctrl Pts',(6.3141746594446,8.12018736172121,0.0544460906262127));
#6138=CARTESIAN_POINT('Ctrl Pts',(6.3174055979117,8.11833493546569,0.10793997063244));
#6139=CARTESIAN_POINT('Ctrl Pts',(6.3206365363788,8.11426759726748,0.161264909122649));
#6140=CARTESIAN_POINT('Ctrl Pts',(6.36279296397899,8.06119804796336,0.857034553651034));
#6141=CARTESIAN_POINT('Ctrl Pts',(6.40494939157917,7.63105440762909,1.52404302381293));
#6142=CARTESIAN_POINT('Ctrl Pts',(6.44710581917936,7.01914833056754,1.8594274721189));
#6143=CARTESIAN_POINT('Ctrl Pts',(6.48926224677956,6.40724225350598,2.19481192042488));
#6144=CARTESIAN_POINT('Ctrl Pts',(6.53141867437976,5.61357373971716,2.19857234687494));
#6145=CARTESIAN_POINT('Ctrl Pts',(6.57357510197995,4.9985170824839,1.86900128670161));
#6146=CARTESIAN_POINT('Ctrl Pts',(6.61573152958014,4.38346042525066,1.53943022652828));
#6147=CARTESIAN_POINT('Ctrl Pts',(6.65788795718032,3.94701562457299,0.876527679731573));
#6148=CARTESIAN_POINT('Ctrl Pts',(6.70004438478051,3.8873554488927,0.181292152195573));
#6149=CARTESIAN_POINT('Ctrl Pts',(6.7422008123807,3.82769527321242,-0.513943375340437));
#6150=CARTESIAN_POINT('Ctrl Pts',(6.78435723998089,4.14481972252953,-1.24151188361575));
#6151=CARTESIAN_POINT('Ctrl Pts',(6.82651366758109,4.69473480272403,-1.67105254511866));
#6152=CARTESIAN_POINT('Ctrl Pts',(6.86867009518128,5.24464988291853,-2.10059320662157));
#6153=CARTESIAN_POINT('Ctrl Pts',(6.91082652278147,6.02735559399041,-2.23210602135209));
#6154=CARTESIAN_POINT('Ctrl Pts',(6.95298295038166,6.68745542899508,-2.00587608712802));
#6155=CARTESIAN_POINT('Ctrl Pts',(6.99513937798185,7.34755526399976,-1.77964615290396));
#6156=CARTESIAN_POINT('Ctrl Pts',(7.03729580558204,7.88504922293722,-1.19567346972529));
#6157=CARTESIAN_POINT('Ctrl Pts',(7.07945223318223,8.05588200786014,-0.519117533452964));
#6158=CARTESIAN_POINT('Ctrl Pts',(7.08994939578065,8.09842023091556,-0.350651700974674));
#6159=CARTESIAN_POINT('Ctrl Pts',(7.10044655837908,8.11822417570459,-0.176445382216928));
#6160=CARTESIAN_POINT('Ctrl Pts',(7.1109437209775,8.11666666562943,-0.00189050366901346));
#6161=CARTESIAN_POINT('Ctrl Pts',(6.8890562790225,8.11363988703895,-0.00031417125408606));
#6162=CARTESIAN_POINT('Ctrl Pts',(6.86915127642532,8.11408383576835,-0.332507738044336));
#6163=CARTESIAN_POINT('Ctrl Pts',(6.84924627382813,8.04036937120591,-0.664514963814514));
#6164=CARTESIAN_POINT('Ctrl Pts',(6.82934127123095,7.8914479510022,-0.958414131147649));
#6165=CARTESIAN_POINT('Ctrl Pts',(6.78718484363076,7.57605009871439,-1.58085760529158));
#6166=CARTESIAN_POINT('Ctrl Pts',(6.74502841603057,6.92331745598877,-2.03237042817807));
#6167=CARTESIAN_POINT('Ctrl Pts',(6.70287198843038,6.22963076710099,-2.1079380230298));
#6168=CARTESIAN_POINT('Ctrl Pts',(6.66071556083018,5.5359440782132,-2.18350561788154));
#6169=CARTESIAN_POINT('Ctrl Pts',(6.61855913322999,4.80130334316326,-1.88312798469853));
#6170=CARTESIAN_POINT('Ctrl Pts',(6.5764027056298,4.35928061515932,-1.34319503362046));
#6171=CARTESIAN_POINT('Ctrl Pts',(6.53424627802961,3.91725788715539,-0.803262082542392));
#6172=CARTESIAN_POINT('Ctrl Pts',(6.49208985042942,3.76785316619748,-0.0237738135692568));
#6173=CARTESIAN_POINT('Ctrl Pts',(6.44993342282923,3.97890537973814,0.641334182842987));
#6174=CARTESIAN_POINT('Ctrl Pts',(6.40777699522904,4.18995759327881,1.30644217925523));
#6175=CARTESIAN_POINT('Ctrl Pts',(6.36562056762885,4.76146674131807,1.85716990310661));
#6176=CARTESIAN_POINT('Ctrl Pts',(6.32346414002865,5.43393253910038,2.04345311368894));
#6177=CARTESIAN_POINT('Ctrl Pts',(6.28130771242846,6.10639833688271,2.22973632427128));
#6178=CARTESIAN_POINT('Ctrl Pts',(6.23915128482827,6.87982078440811,2.05157502158459));
#6179=CARTESIAN_POINT('Ctrl Pts',(6.19699485722808,7.40301854703335,1.58986538889771));
#6180=CARTESIAN_POINT('Ctrl Pts',(6.16101533115955,7.84955561411832,1.19580700418601));
#6181=CARTESIAN_POINT('Ctrl Pts',(6.12503580509103,8.11382342309418,0.595205672810865));
#6182=CARTESIAN_POINT('Ctrl Pts',(6.0890562790225,8.11876545586576,-0.0015626071037439));
#6183=CARTESIAN_POINT('Origin',(6.,6.,0.));
#6184=CARTESIAN_POINT('',(5.2890562790225,8.11812209636794,0.00175000182231128));
#6185=CARTESIAN_POINT('',(5.51094372097749,8.11412427934883,0.00104751275875566));
#6186=CARTESIAN_POINT('',(6.,8.117,2.59257727379495E-16));
#6187=CARTESIAN_POINT('Ctrl Pts',(5.51094372097749,8.11412427934883,0.00104751275875566));
#6188=CARTESIAN_POINT('Ctrl Pts',(5.52790276051011,8.11540248649808,0.28391388762074));
#6189=CARTESIAN_POINT('Ctrl Pts',(5.54486180004273,8.06257424903286,0.566322454846834));
#6190=CARTESIAN_POINT('Ctrl Pts',(5.56182083957536,7.95336598668525,0.824921308871607));
#6191=CARTESIAN_POINT('Ctrl Pts',(5.60397726717555,7.6818983604589,1.46774095949028));
#6192=CARTESIAN_POINT('Ctrl Pts',(5.64613369477574,7.06205302422545,1.96343805423379));
#6193=CARTESIAN_POINT('Ctrl Pts',(5.68829012237593,6.37527786348045,2.08693564082625));
#6194=CARTESIAN_POINT('Ctrl Pts',(5.73044654997612,5.68850270273544,2.21043322741871));
#6195=CARTESIAN_POINT('Ctrl Pts',(5.77260297757631,4.93479771747889,1.9617313058601));
#6196=CARTESIAN_POINT('Ctrl Pts',(5.8147594051765,4.45639130242119,1.45375583662744));
#6197=CARTESIAN_POINT('Ctrl Pts',(5.85691583277669,3.9779848873635,0.94578036739478));
#6198=CARTESIAN_POINT('Ctrl Pts',(5.89907226037688,3.77487704250467,0.178531350488057));
#6199=CARTESIAN_POINT('Ctrl Pts',(5.94122868797708,3.93929121476205,-0.499612996440685));
#6200=CARTESIAN_POINT('Ctrl Pts',(5.98338511557727,4.10370538701942,-1.17775734336943));
#6201=CARTESIAN_POINT('Ctrl Pts',(6.02554154317746,4.635641576393,-1.7667970203202));
#6202=CARTESIAN_POINT('Ctrl Pts',(6.06769797077765,5.29356805397195,-1.99927180478301));
#6203=CARTESIAN_POINT('Ctrl Pts',(6.10985439837784,5.9514945315509,-2.23174658924581));
#6204=CARTESIAN_POINT('Ctrl Pts',(6.15201082597803,6.73541129733521,-2.10765648122066));
#6205=CARTESIAN_POINT('Ctrl Pts',(6.19416725357822,7.28937195109038,-1.68334601776064));
#6206=CARTESIAN_POINT('Ctrl Pts',(6.23309274271131,7.80087614239452,-1.29155541132901));
#6207=CARTESIAN_POINT('Ctrl Pts',(6.27201823184441,8.1163219073926,-0.643799743076592));
#6208=CARTESIAN_POINT('Ctrl Pts',(6.3109437209775,8.11989110689617,0.00093137289447728));
#6209=CARTESIAN_POINT('Ctrl Pts',(6.0890562790225,8.11876545586576,-0.0015626071037439));
#6210=CARTESIAN_POINT('Ctrl Pts',(6.08287937749084,8.11961389532931,-0.104014732104856));
#6211=CARTESIAN_POINT('Ctrl Pts',(6.07670247595917,8.1128191182144,-0.206353883984291));
#6212=CARTESIAN_POINT('Ctrl Pts',(6.07052557442751,8.09799122284675,-0.307515571951035));
#6213=CARTESIAN_POINT('Ctrl Pts',(6.02836914682732,7.99679305830984,-0.997928937425843));
#6214=CARTESIAN_POINT('Ctrl Pts',(5.98621271922713,7.52142365151097,-1.63349770568842));
#6215=CARTESIAN_POINT('Ctrl Pts',(5.94405629162694,6.8877299348249,-1.92563458655846));
#6216=CARTESIAN_POINT('Ctrl Pts',(5.90189986402674,6.25403621813882,-2.21777146742851));
#6217=CARTESIAN_POINT('Ctrl Pts',(5.85974343642655,5.46201819156553,-2.16647646090602));
#6218=CARTESIAN_POINT('Ctrl Pts',(5.81758700882636,4.87130072573482,-1.79504065313509));
#6219=CARTESIAN_POINT('Ctrl Pts',(5.77543058122617,4.28058325990411,-1.42360484536416));
#6220=CARTESIAN_POINT('Ctrl Pts',(5.73327415362598,3.89116635481596,-0.732028236344795));
#6221=CARTESIAN_POINT('Ctrl Pts',(5.69111772602579,3.8798692234361,-0.0343291188489477));
#6222=CARTESIAN_POINT('Ctrl Pts',(5.6489612984256,3.86857209205625,0.6633699986469));
#6223=CARTESIAN_POINT('Ctrl Pts',(5.60680487082541,4.23539473438468,1.36719162461923));
#6224=CARTESIAN_POINT('Ctrl Pts',(5.56464844322521,4.81377712165265,1.75755747587944));
#6225=CARTESIAN_POINT('Ctrl Pts',(5.52249201562502,5.39215950892061,2.14792332713965));
#6226=CARTESIAN_POINT('Ctrl Pts',(5.48033558802483,6.18210164112811,2.22483340368774));
#6227=CARTESIAN_POINT('Ctrl Pts',(5.43817916042464,6.82492123129587,1.95336580299024));
#6228=CARTESIAN_POINT('Ctrl Pts',(5.39602273282445,7.46774082146363,1.68189820229274));
#6229=CARTESIAN_POINT('Ctrl Pts',(5.35386630522426,7.96343786959165,1.06205292434967));
#6230=CARTESIAN_POINT('Ctrl Pts',(5.31170987762407,8.08693544457034,0.375277828189158));
#6231=CARTESIAN_POINT('Ctrl Pts',(5.30415867809021,8.10905674098226,0.252260388590747));
#6232=CARTESIAN_POINT('Ctrl Pts',(5.29660747855636,8.11923595551276,0.127095494664423));
#6233=CARTESIAN_POINT('Ctrl Pts',(5.2890562790225,8.11812209636794,0.00175000182231128));
#6234=CARTESIAN_POINT('Origin',(6.,6.,0.));
#6235=CARTESIAN_POINT('',(4.4890562790225,8.11359750489683,-5.40837440764219E-5));
#6236=CARTESIAN_POINT('',(4.71094372097749,8.11619797856316,-0.00185818891683977));
#6237=CARTESIAN_POINT('',(6.,8.117,2.59257727379495E-16));
#6238=CARTESIAN_POINT('Ctrl Pts',(4.71094372097749,8.11619797856316,-0.00185818891683977));
#6239=CARTESIAN_POINT('Ctrl Pts',(4.74163086157564,8.11180556396272,0.508719219713788));
#6240=CARTESIAN_POINT('Ctrl Pts',(4.77231800217378,7.92596018761809,1.02216466154014));
#6241=CARTESIAN_POINT('Ctrl Pts',(4.80300514277192,7.58986553840906,1.40301867897351));
#6242=CARTESIAN_POINT('Ctrl Pts',(4.84516157037211,7.12815586230291,1.9262164908004));
#6243=CARTESIAN_POINT('Ctrl Pts',(4.8873179979723,6.38289782953163,2.19918959419595));
#6244=CARTESIAN_POINT('Ctrl Pts',(4.92947442557249,5.69248439913017,2.09799142014236));
#6245=CARTESIAN_POINT('Ctrl Pts',(4.97163085317269,5.00207096872872,1.99679324608877));
#6246=CARTESIAN_POINT('Ctrl Pts',(5.01378728077288,4.3665021406971,1.52142379458605));
#6247=CARTESIAN_POINT('Ctrl Pts',(5.05594370837307,4.07436523235441,0.887730018307272));
#6248=CARTESIAN_POINT('Ctrl Pts',(5.09810013597325,3.78222832401172,0.254036242028489));
#6249=CARTESIAN_POINT('Ctrl Pts',(5.14025656357344,3.83352333535799,-0.537981859026349));
#6250=CARTESIAN_POINT('Ctrl Pts',(5.18241299117363,4.20495917805882,-1.12869938040828));
#6251=CARTESIAN_POINT('Ctrl Pts',(5.22456941877383,4.57639502075965,-1.71941690179022));
#6252=CARTESIAN_POINT('Ctrl Pts',(5.26672584637402,5.26797169481504,-2.10883384349925));
#6253=CARTESIAN_POINT('Ctrl Pts',(5.30888227397421,5.96567087792268,-2.12013097594151));
#6254=CARTESIAN_POINT('Ctrl Pts',(5.3510387015744,6.66337006103032,-2.13142810838377));
#6255=CARTESIAN_POINT('Ctrl Pts',(5.39319512917459,7.36719175319021,-1.76460543155926));
#6256=CARTESIAN_POINT('Ctrl Pts',(5.43535155677478,7.75755764116054,-1.18622298990009));
#6257=CARTESIAN_POINT('Ctrl Pts',(5.46054894484235,7.99088388172379,-0.8405170640524));
#6258=CARTESIAN_POINT('Ctrl Pts',(5.48574633290992,8.11222514576236,-0.419229461356099));
#6259=CARTESIAN_POINT('Ctrl Pts',(5.51094372097749,8.11412427934883,0.00104751275875566));
#6260=CARTESIAN_POINT('Ctrl Pts',(5.2890562790225,8.11812209636794,0.00175000182231128));
#6261=CARTESIAN_POINT('Ctrl Pts',(5.25445105095617,8.11301756303291,-0.572676531000783));
#6262=CARTESIAN_POINT('Ctrl Pts',(5.21984582288983,7.87074087424131,-1.15089592264707));
#6263=CARTESIAN_POINT('Ctrl Pts',(5.1852405948235,7.45375569991587,-1.54360855241751));
#6264=CARTESIAN_POINT('Ctrl Pts',(5.14308416722331,6.94578027845333,-2.02201492248574));
#6265=CARTESIAN_POINT('Ctrl Pts',(5.10092773962311,6.17853133369889,-2.22512274824425));
#6266=CARTESIAN_POINT('Ctrl Pts',(5.05877131202292,5.500387050543,-2.06070859144841));
#6267=CARTESIAN_POINT('Ctrl Pts',(5.01661488442273,4.82224276738711,-1.89629443465257));
#6268=CARTESIAN_POINT('Ctrl Pts',(4.97445845682254,4.23320314582978,-1.36435829530238));
#6269=CARTESIAN_POINT('Ctrl Pts',(4.93230202922235,4.00072838322897,-0.706431879594986));
#6270=CARTESIAN_POINT('Ctrl Pts',(4.89014560162216,3.76825362062816,-0.0485054638875976));
#6271=CARTESIAN_POINT('Ctrl Pts',(4.84798917402197,3.89234371698386,0.735411228176989));
#6272=CARTESIAN_POINT('Ctrl Pts',(4.80583274642178,4.31665414054163,1.28937182983757));
#6273=CARTESIAN_POINT('Ctrl Pts',(4.76367631882158,4.74096456409941,1.84333243149815));
#6274=CARTESIAN_POINT('Ctrl Pts',(4.7215198912214,5.46549531485925,2.16733694275472));
#6275=CARTESIAN_POINT('Ctrl Pts',(4.6793634636212,6.1612648939573,2.11426739844126));
#6276=CARTESIAN_POINT('Ctrl Pts',(4.63720703602101,6.85703447305535,2.0611978541278));
#6277=CARTESIAN_POINT('Ctrl Pts',(4.59505060842082,7.5240428804916,1.63105425424432));
#6278=CARTESIAN_POINT('Ctrl Pts',(4.55289418082063,7.85942729725793,1.01914823472655));
#6279=CARTESIAN_POINT('Ctrl Pts',(4.53161488022125,8.02871929439777,0.710276423970282));
#6280=CARTESIAN_POINT('Ctrl Pts',(4.51033557962188,8.11351589694749,0.355092863157482));
#6281=CARTESIAN_POINT('Ctrl Pts',(4.4890562790225,8.11359750489683,-5.40837440764219E-5));
#6282=CARTESIAN_POINT('Origin',(6.,6.,0.));
#6283=CARTESIAN_POINT('',(3.6890562790225,8.11831511071496,-0.001702946356694));
#6284=CARTESIAN_POINT('',(3.91094372097749,8.12014460849304,0.000668395368594085));
#6285=CARTESIAN_POINT('',(6.,8.117,2.59257727379495E-16));
#6286=CARTESIAN_POINT('Ctrl Pts',(3.91094372097749,8.12014460849304,0.000668395368594085));
#6287=CARTESIAN_POINT('Ctrl Pts',(3.91320253504096,8.12030022770606,0.0380697174170374));
#6288=CARTESIAN_POINT('Ctrl Pts',(3.91546134910444,8.1193954443398,0.0754633589122573));
#6289=CARTESIAN_POINT('Ctrl Pts',(3.91772016316791,8.11740647361435,0.112799243186508));
#6290=CARTESIAN_POINT('Ctrl Pts',(3.9598765907681,8.08028615382247,0.80960183873867));
#6291=CARTESIAN_POINT('Ctrl Pts',(4.00203301836829,7.66553193262247,1.48628698456753));
#6292=CARTESIAN_POINT('Ctrl Pts',(4.04418944596848,7.06146772201725,1.83559802758844));
#6293=CARTESIAN_POINT('Ctrl Pts',(4.08634587356867,6.45740351141202,2.18490907060935));
#6294=CARTESIAN_POINT('Ctrl Pts',(4.12850230116887,5.66402931140155,2.20684601082232));
#6295=CARTESIAN_POINT('Ctrl Pts',(4.17065872876906,5.04158577872288,1.89144812887443));
#6296=CARTESIAN_POINT('Ctrl Pts',(4.21281515636925,4.41914224604421,1.57605024692654));
#6297=CARTESIAN_POINT('Ctrl Pts',(4.25497158396943,3.96762938069734,0.923317542817797));
#6298=CARTESIAN_POINT('Ctrl Pts',(4.29712801156963,3.8920617787392,0.22963078869555));
#6299=CARTESIAN_POINT('Ctrl Pts',(4.33928443916982,3.81649417678106,-0.464055965426697));
#6300=CARTESIAN_POINT('Ctrl Pts',(4.38144086677001,4.11687183821165,-1.19869676956244));
#6301=CARTESIAN_POINT('Ctrl Pts',(4.4235972943702,4.65680484006513,-1.64071953913431));
#6302=CARTESIAN_POINT('Ctrl Pts',(4.46575372197039,5.19673784191862,-2.08274230870617));
#6303=CARTESIAN_POINT('Ctrl Pts',(4.50791014957058,5.97622618419501,-2.23214704371415));
#6304=CARTESIAN_POINT('Ctrl Pts',(4.55006657717077,6.64133424315417,-2.0210948103261));
#6305=CARTESIAN_POINT('Ctrl Pts',(4.59222300477096,7.30644230211334,-1.81004257693804));
#6306=CARTESIAN_POINT('Ctrl Pts',(4.63437943237115,7.85717007775528,-1.23853337515395));
#6307=CARTESIAN_POINT('Ctrl Pts',(4.67653585997135,8.04345330585575,-0.566067514132789));
#6308=CARTESIAN_POINT('Ctrl Pts',(4.6880051469734,8.09413444579994,-0.383113113150845));
#6309=CARTESIAN_POINT('Ctrl Pts',(4.69947443397545,8.11783963896887,-0.192685966357322));
#6310=CARTESIAN_POINT('Ctrl Pts',(4.71094372097749,8.11619797856316,-0.00185818891683977));
#6311=CARTESIAN_POINT('Ctrl Pts',(4.4890562790225,8.11359750489683,-5.40837440764219E-5));
#6312=CARTESIAN_POINT('Ctrl Pts',(4.46817915202169,8.11367757047581,-0.348488839848436));
#6313=CARTESIAN_POINT('Ctrl Pts',(4.44730202502087,8.03221456672079,-0.696888352951045));
#6314=CARTESIAN_POINT('Ctrl Pts',(4.42642489802006,7.86900111094028,-1.00148282333643));
#6315=CARTESIAN_POINT('Ctrl Pts',(4.38426847041987,7.53943008175988,-1.61653942272961));
#6316=CARTESIAN_POINT('Ctrl Pts',(4.34211204281967,6.87652759730266,-2.05298418236391));
#6317=CARTESIAN_POINT('Ctrl Pts',(4.29995561521948,6.18129213514676,-2.11264435243372));
#6318=CARTESIAN_POINT('Ctrl Pts',(4.25779918761929,5.48605667299086,-2.17230452250352));
#6319=CARTESIAN_POINT('Ctrl Pts',(4.2156427600191,4.75848823313627,-1.85518010300883));
#6320=CARTESIAN_POINT('Ctrl Pts',(4.17348633241891,4.32894761202748,-1.30526507452847));
#6321=CARTESIAN_POINT('Ctrl Pts',(4.13132990481872,3.89940699091868,-0.755350046048115));
#6322=CARTESIAN_POINT('Ctrl Pts',(4.08917347721853,3.76789418855569,0.0273555914179174));
#6323=CARTESIAN_POINT('Ctrl Pts',(4.04701704961834,3.99412410150505,0.687455364346652));
#6324=CARTESIAN_POINT('Ctrl Pts',(4.00486062201815,4.22035401445442,1.34755513727539));
#6325=CARTESIAN_POINT('Ctrl Pts',(3.96270419441795,4.80432664271614,1.88504904566683));
#6326=CARTESIAN_POINT('Ctrl Pts',(3.92054776681776,5.48088251536499,2.05588181452455));
#6327=CARTESIAN_POINT('Ctrl Pts',(3.87839133921757,6.15743838801383,2.22671458338228));
#6328=CARTESIAN_POINT('Ctrl Pts',(3.83623491161738,6.9265775050498,2.03088621270629));
#6329=CARTESIAN_POINT('Ctrl Pts',(3.7940784840172,7.43906342717357,1.55731482067357));
#6330=CARTESIAN_POINT('Ctrl Pts',(3.7590710823523,7.86464029752753,1.1640532261399));
#6331=CARTESIAN_POINT('Ctrl Pts',(3.7240636806874,8.11323120292733,0.579262293111433));
#6332=CARTESIAN_POINT('Ctrl Pts',(3.6890562790225,8.11831511071496,-0.001702946356694));
#6333=CARTESIAN_POINT('Origin',(6.,6.,0.));
#6334=CARTESIAN_POINT('',(2.8890562790225,8.11858235385061,0.0016251550495));
#6335=CARTESIAN_POINT('',(3.11094372097749,8.11439370554494,0.0012559944889576));
#6336=CARTESIAN_POINT('',(6.,8.117,2.59257727379495E-16));
#6337=CARTESIAN_POINT('Ctrl Pts',(3.11094372097749,8.11439370554494,0.0012559944889576));
#6338=CARTESIAN_POINT('Ctrl Pts',(3.12693063610649,8.11584979458628,0.267822697439219));
#6339=CARTESIAN_POINT('Ctrl Pts',(3.14291755123548,8.06908489296678,0.533897341735394));
#6340=CARTESIAN_POINT('Ctrl Pts',(3.15890446636447,7.97174688398804,0.779966710265086));
#6341=CARTESIAN_POINT('Ctrl Pts',(3.20106089396466,7.71507305447496,1.42883520273831));
#6342=CARTESIAN_POINT('Ctrl Pts',(3.24321732156485,7.10674333009371,1.93859867439931));
#6343=CARTESIAN_POINT('Ctrl Pts',(3.28537374916504,6.42297680060745,2.07779317305597));
#6344=CARTESIAN_POINT('Ctrl Pts',(3.32753017676523,5.73921027112117,2.21698767171264));
#6345=CARTESIAN_POINT('Ctrl Pts',(3.36968660436542,4.98000693652988,1.98561319736497));
#6346=CARTESIAN_POINT('Ctrl Pts',(3.41184303196562,4.49009178017005,1.48872798437086));
#6347=CARTESIAN_POINT('Ctrl Pts',(3.45399945956581,4.00017662381023,0.99184277137675));
#6348=CARTESIAN_POINT('Ctrl Pts',(3.496155887166,3.77954964568186,0.229446819736206));
#6349=CARTESIAN_POINT('Ctrl Pts',(3.53831231476619,3.92838905611583,-0.452285242886036));
#6350=CARTESIAN_POINT('Ctrl Pts',(3.58046874236638,4.0772284665498,-1.13401730550828));
#6351=CARTESIAN_POINT('Ctrl Pts',(3.62262516996657,4.59553426554611,-1.73508547911222));
#6352=CARTESIAN_POINT('Ctrl Pts',(3.66478159756676,5.24796375931615,-1.98256786428093));
#6353=CARTESIAN_POINT('Ctrl Pts',(3.70693802516695,5.90039325308621,-2.23005024944964));
#6354=CARTESIAN_POINT('Ctrl Pts',(3.74909445276714,6.68694644163,-2.12394684618312));
#6355=CARTESIAN_POINT('Ctrl Pts',(3.79125088036733,7.25047982671001,-1.71243512191212));
#6356=CARTESIAN_POINT('Ctrl Pts',(3.83114849390405,7.78381812155308,-1.32297290522469));
#6357=CARTESIAN_POINT('Ctrl Pts',(3.87104610744077,8.11739589388198,-0.659954148550725));
#6358=CARTESIAN_POINT('Ctrl Pts',(3.91094372097749,8.12014460849304,0.000668395368594085));
#6359=CARTESIAN_POINT('Ctrl Pts',(3.6890562790225,8.11831511071496,-0.001702946356694));
#6360=CARTESIAN_POINT('Ctrl Pts',(3.68190725308721,8.11935331940506,-0.120344586893705));
#6361=CARTESIAN_POINT('Ctrl Pts',(3.67475822715191,8.11023639929483,-0.238826682073759));
#6362=CARTESIAN_POINT('Ctrl Pts',(3.66760920121662,8.09039782422567,-0.355485491400828));
#6363=CARTESIAN_POINT('Ctrl Pts',(3.62545277361643,7.97341357194241,-1.04339999805302));
#6364=CARTESIAN_POINT('Ctrl Pts',(3.58329634601624,7.48361234016431,-1.66791459796793));
#6365=CARTESIAN_POINT('Ctrl Pts',(3.54113991841605,6.84339399694864,-1.94546127284174));
#6366=CARTESIAN_POINT('Ctrl Pts',(3.49898349081586,6.20317565373296,-2.22300794771556));
#6367=CARTESIAN_POINT('Ctrl Pts',(3.45682706321567,5.41254019907969,-2.15358669754827));
#6368=CARTESIAN_POINT('Ctrl Pts',(3.41467063561547,4.83048473098684,-1.76871903748089));
#6369=CARTESIAN_POINT('Ctrl Pts',(3.37251420801528,4.24842926289399,-1.38385137741351));
#6370=CARTESIAN_POINT('Ctrl Pts',(3.33035778041509,3.87495378136155,-0.683537307446053));
#6371=CARTESIAN_POINT('Ctrl Pts',(3.2882013528149,3.87963911310041,0.014237535530621));
#6372=CARTESIAN_POINT('Ctrl Pts',(3.24604492521471,3.88432444483927,0.712012378507305));
#6373=CARTESIAN_POINT('Ctrl Pts',(3.20388849761452,4.26717058984945,1.40724799449321));
#6374=CARTESIAN_POINT('Ctrl Pts',(3.16173207001433,4.85434186418734,1.78426467613756));
#6375=CARTESIAN_POINT('Ctrl Pts',(3.11957564241414,5.44151313852524,2.16128135778191));
#6376=CARTESIAN_POINT('Ctrl Pts',(3.07741921481395,6.23300954219084,2.22007910508473));
#6377=CARTESIAN_POINT('Ctrl Pts',(3.03526278721375,6.86944305335818,1.93396012732273));
#6378=CARTESIAN_POINT('Ctrl Pts',(2.99310635961356,7.50587656452552,1.64784114956073));
#6379=CARTESIAN_POINT('Ctrl Pts',(2.95094993201337,7.9872471831946,1.01680544673392));
#6380=CARTESIAN_POINT('Ctrl Pts',(2.90879350441318,8.0949830580151,0.327382016861069));
#6381=CARTESIAN_POINT('Ctrl Pts',(2.90221442928295,8.11179668419298,0.219788257145721));
#6382=CARTESIAN_POINT('Ctrl Pts',(2.89563535415273,8.11951014375889,0.110772418640964));
#6383=CARTESIAN_POINT('Ctrl Pts',(2.8890562790225,8.11858235385061,0.00162515504950001));
#6384=CARTESIAN_POINT('Origin',(6.,6.,0.));
#6385=CARTESIAN_POINT('',(2.0890562790225,8.11361510105375,0.000206967465626595));
#6386=CARTESIAN_POINT('',(2.31094372097749,8.11574927685536,-0.00178855551209614));
#6387=CARTESIAN_POINT('',(6.,8.117,2.59257727379495E-16));
#6388=CARTESIAN_POINT('Ctrl Pts',(2.31094372097749,8.11574927685536,-0.00178855551209614));
#6389=CARTESIAN_POINT('Ctrl Pts',(2.340658737172,8.1117226042171,0.492880798811412));
#6390=CARTESIAN_POINT('Ctrl Pts',(2.37037375336652,7.93849788809162,0.990091593431114));
#6391=CARTESIAN_POINT('Ctrl Pts',(2.40008876956103,7.62158202934387,1.36623773853909));
#6392=CARTESIAN_POINT('Ctrl Pts',(2.44224519716122,7.17197633614156,1.89987290903797));
#6393=CARTESIAN_POINT('Ctrl Pts',(2.48440162476141,6.43316573578127,2.18984315988211));
#6394=CARTESIAN_POINT('Ctrl Pts',(2.5265580523616,5.74061565324586,2.1044841666656));
#6395=CARTESIAN_POINT('Ctrl Pts',(2.5687144799618,5.04806557071046,2.01912517344909));
#6396=CARTESIAN_POINT('Ctrl Pts',(2.61087090756198,4.40177600599992,1.55843693617193));
#6397=CARTESIAN_POINT('Ctrl Pts',(2.65302733516217,4.09520215168382,0.931600236700099));
#6398=CARTESIAN_POINT('Ctrl Pts',(2.69518376276237,3.78862829736771,0.30476353722827));
#6399=CARTESIAN_POINT('Ctrl Pts',(2.73734019036256,3.82177015344603,-0.488221624438216));
#6400=CARTESIAN_POINT('Ctrl Pts',(2.77949661796275,4.17957927904964,-1.08729124041551));
#6401=CARTESIAN_POINT('Ctrl Pts',(2.82165304556294,4.53738840465323,-1.6863608563928));
#6402=CARTESIAN_POINT('Ctrl Pts',(2.86380947316313,5.21986479978211,-2.09151492668089));
#6403=CARTESIAN_POINT('Ctrl Pts',(2.90596590076332,5.91712222865987,-2.11878859712663));
#6404=CARTESIAN_POINT('Ctrl Pts',(2.94812232836351,6.61437965753764,-2.14606226757236));
#6405=CARTESIAN_POINT('Ctrl Pts',(2.99027875596371,7.32641812016429,-1.79545553817573));
#6406=CARTESIAN_POINT('Ctrl Pts',(3.0324351835639,7.72992838415516,-1.22616541683467));
#6407=CARTESIAN_POINT('Ctrl Pts',(3.0586046960351,7.98041609117609,-0.87276628464403));
#6408=CARTESIAN_POINT('Ctrl Pts',(3.0847742085063,8.11201018502086,-0.435095897103462));
#6409=CARTESIAN_POINT('Ctrl Pts',(3.11094372097749,8.11439370554494,0.0012559944889576));
#6410=CARTESIAN_POINT('Ctrl Pts',(2.8890562790225,8.11858235385061,0.00162515504950001));
#6411=CARTESIAN_POINT('Ctrl Pts',(2.85347892655254,8.11356518837803,-0.588605324320554));
#6412=CARTESIAN_POINT('Ctrl Pts',(2.81790157408257,7.85585450325349,-1.18267902888964));
#6413=CARTESIAN_POINT('Ctrl Pts',(2.78232422161261,7.41802088245732,-1.57649921610984));
#6414=CARTESIAN_POINT('Ctrl Pts',(2.74016779401242,6.89922170110715,-2.04314586228899));
#6415=CARTESIAN_POINT('Ctrl Pts',(2.69801136641222,6.12752220743493,-2.22862799772838));
#6416=CARTESIAN_POINT('Ctrl Pts',(2.65585493881203,5.45332140955135,-2.04872533765658));
#6417=CARTESIAN_POINT('Ctrl Pts',(2.61369851121184,4.77912061166776,-1.86882267758478));
#6418=CARTESIAN_POINT('Ctrl Pts',(2.57154208361165,4.20241850957281,-1.3235352220018));
#6419=CARTESIAN_POINT('Ctrl Pts',(2.52938565601146,3.9850733075603,-0.660456982788181));
#6420=CARTESIAN_POINT('Ctrl Pts',(2.48722922841127,3.7677281055478,0.00262125642543298));
#6421=CARTESIAN_POINT('Ctrl Pts',(2.44507280081108,3.90973980361775,0.783490279269671));
#6422=CARTESIAN_POINT('Ctrl Pts',(2.40291637321089,4.34662636274209,1.32758752401669));
#6423=CARTESIAN_POINT('Ctrl Pts',(2.36075994561069,4.78351292186642,1.87168476876371));
#6424=CARTESIAN_POINT('Ctrl Pts',(2.31860351801051,5.51527434204514,2.17901023541351));
#6425=CARTESIAN_POINT('Ctrl Pts',(2.27644709041031,6.20964595300729,2.11001931653322));
#6426=CARTESIAN_POINT('Ctrl Pts',(2.23429066281012,6.90401756396943,2.04102839765292));
#6427=CARTESIAN_POINT('Ctrl Pts',(2.19213423520993,7.56099936571499,1.59572109324253));
#6428=CARTESIAN_POINT('Ctrl Pts',(2.14997780760974,7.882281240332,0.976294204819711));
#6429=CARTESIAN_POINT('Ctrl Pts',(2.129670631414,8.03704595849608,0.677910027609945));
#6430=CARTESIAN_POINT('Ctrl Pts',(2.10936345521825,8.11391332031157,0.33912234063746));
#6431=CARTESIAN_POINT('Ctrl Pts',(2.0890562790225,8.11361510105375,0.000206967465626595));
#6432=CARTESIAN_POINT('Origin',(6.,6.,0.));
#6433=CARTESIAN_POINT('',(1.2890562790225,8.11784406625472,-0.00180833638339553));
#6434=CARTESIAN_POINT('',(1.51094372097749,8.12031955932164,0.000387557394038608));
#6435=CARTESIAN_POINT('',(6.,8.117,2.59257727379495E-16));
#6436=CARTESIAN_POINT('Ctrl Pts',(1.51094372097749,8.12031955932164,0.000387557394038608));
#6437=CARTESIAN_POINT('Ctrl Pts',(1.51223041063733,8.12037363613379,0.0216878003480682));
#6438=CARTESIAN_POINT('Ctrl Pts',(1.51351710029718,8.1200801867452,0.0429865167899391));
#6439=CARTESIAN_POINT('Ctrl Pts',(1.51480378995702,8.11943460408254,0.064274553967799));
#6440=CARTESIAN_POINT('Ctrl Pts',(1.55696021755721,8.09828307109983,0.761744679086335));
#6441=CARTESIAN_POINT('Ctrl Pts',(1.5991166451574,7.6991356766239,1.44775119682358));
#6442=CARTESIAN_POINT('Ctrl Pts',(1.64127307275759,7.10323019476973,1.81080550658276));
#6443=CARTESIAN_POINT('Ctrl Pts',(1.68342950035778,6.50732471291556,2.17385981634195));
#6444=CARTESIAN_POINT('Ctrl Pts',(1.72558592795797,5.71466114368315,2.21396191812306));
#6445=CARTESIAN_POINT('Ctrl Pts',(1.76774235555816,5.08515730617276,1.91290271660692));
#6446=CARTESIAN_POINT('Ctrl Pts',(1.80989878315835,4.45565346866237,1.61184351509078));
#6447=CARTESIAN_POINT('Ctrl Pts',(1.85205521075855,3.98930936287399,0.969623010277392));
#6448=CARTESIAN_POINT('Ctrl Pts',(1.89421163835874,3.89787396725924,0.277848933787433));
#6449=CARTESIAN_POINT('Ctrl Pts',(1.93636806595893,3.80643857164448,-0.413925142702522));
#6450=CARTESIAN_POINT('Ctrl Pts',(1.97852449355912,4.08991188620336,-1.15525279086904));
#6451=CARTESIAN_POINT('Ctrl Pts',(2.02068092115931,4.61957955486217,-1.60952576319302));
#6452=CARTESIAN_POINT('Ctrl Pts',(2.0628373487595,5.14924722352099,-2.06379873551699));
#6453=CARTESIAN_POINT('Ctrl Pts',(2.10499377635969,5.92510924627976,-2.23101703199842));
#6454=CARTESIAN_POINT('Ctrl Pts',(2.14715020395988,6.59487659525853,-2.03525322753699));
#6455=CARTESIAN_POINT('Ctrl Pts',(2.18930663156007,7.2646439442373,-1.83948942307556));
#6456=CARTESIAN_POINT('Ctrl Pts',(2.23146305916027,7.82831661943608,-1.28074351767128));
#6457=CARTESIAN_POINT('Ctrl Pts',(2.27361948676046,8.0299525640133,-0.612720519892336));
#6458=CARTESIAN_POINT('Ctrl Pts',(2.28606089816614,8.08946035163823,-0.415570300650682));
#6459=CARTESIAN_POINT('Ctrl Pts',(2.29850230957181,8.11743520866037,-0.208902188115691));
#6460=CARTESIAN_POINT('Ctrl Pts',(2.31094372097749,8.11574927685536,-0.00178855551209614));
#6461=CARTESIAN_POINT('Ctrl Pts',(2.0890562790225,8.11361510105375,0.000206967465626595));
#6462=CARTESIAN_POINT('Ctrl Pts',(2.06720702761806,8.11329423578549,-0.36444477543956));
#6463=CARTESIAN_POINT('Ctrl Pts',(2.04535777621361,8.02364329923712,-0.729244333175282));
#6464=CARTESIAN_POINT('Ctrl Pts',(2.02350852480917,7.84557375391058,-1.04402616427932));
#6465=CARTESIAN_POINT('Ctrl Pts',(1.98135209720898,7.5020024453837,-1.65137317252026));
#6466=CARTESIAN_POINT('Ctrl Pts',(1.93919566960879,6.8292778808415,-2.07252071656688));
#6467=CARTESIAN_POINT('Ctrl Pts',(1.8970392420086,6.13285838710263,-2.11624224665416));
#6468=CARTESIAN_POINT('Ctrl Pts',(1.8548828144084,5.43643889336376,-2.15996377674144));
#6469=CARTESIAN_POINT('Ctrl Pts',(1.81272638680821,4.71632447042824,-1.82625929286939));
#6470=CARTESIAN_POINT('Ctrl Pts',(1.77056995920802,4.29949129246079,-1.26665052430996));
#6471=CARTESIAN_POINT('Ctrl Pts',(1.72841353160783,3.88265811449333,-0.707041755750532));
#6472=CARTESIAN_POINT('Ctrl Pts',(1.68625710400764,3.76910618149396,0.0784712974962866));
#6473=CARTESIAN_POINT('Ctrl Pts',(1.64410067640745,4.0103951285527,0.733216236499067));
#6474=CARTESIAN_POINT('Ctrl Pts',(1.60194424880726,4.25168407561144,1.38796117550185));
#6475=CARTESIAN_POINT('Ctrl Pts',(1.55978782120707,4.84781390272829,1.9119380002606));
#6476=CARTESIAN_POINT('Ctrl Pts',(1.51763139360688,5.5281048754434,2.0672312925924));
#6477=CARTESIAN_POINT('Ctrl Pts',(1.47547496600669,6.20839584815852,2.2225245849242));
#6478=CARTESIAN_POINT('Ctrl Pts',(1.4333185384065,6.97284796647189,2.00913434482906));
#6479=CARTESIAN_POINT('Ctrl Pts',(1.3911621108063,7.47435325973884,1.52394851450554));
#6480=CARTESIAN_POINT('Ctrl Pts',(1.35712683354504,7.87924695391555,1.13223044923417));
#6481=CARTESIAN_POINT('Ctrl Pts',(1.32309155628377,8.11274534553969,0.563349235438652));
#6482=CARTESIAN_POINT('Ctrl Pts',(1.2890562790225,8.11784406625472,-0.00180833638339553));
#6483=CARTESIAN_POINT('Origin',(6.,6.,0.));
#6484=CARTESIAN_POINT('',(0.489056279022499,8.11901932033641,0.00140296810865748));
#6485=CARTESIAN_POINT('',(0.710943720977492,8.11470858782477,0.00143578057856379));
#6486=CARTESIAN_POINT('',(6.,8.117,2.59257727379495E-16));
#6487=CARTESIAN_POINT('',(0.,4.38007430561128,1.36291222925734));
#6488=CARTESIAN_POINT('Ctrl Pts',(0.489056279022499,8.11901932033641,0.00140296810865748));
#6489=CARTESIAN_POINT('Ctrl Pts',(0.452506802148906,8.11421578579102,-0.604476942141384));
#6490=CARTESIAN_POINT('Ctrl Pts',(0.415957325275312,7.84046069996979,-1.21398493528909));
#6491=CARTESIAN_POINT('Ctrl Pts',(0.379407848401719,7.38152818454084,-1.60833829653761));
#6492=CARTESIAN_POINT('Ctrl Pts',(0.337251420801528,6.85219214432977,-2.0631882792025));
#6493=CARTESIAN_POINT('Ctrl Pts',(0.295094993201336,6.07650567520028,-2.23180772089687));
#6494=CARTESIAN_POINT('Ctrl Pts',(0.252938565601145,5.40656319001716,-2.0360753062762));
#6495=CARTESIAN_POINT('Ctrl Pts',(0.210782138000954,4.73662070483403,-1.84034289165553));
#6496=CARTESIAN_POINT('Ctrl Pts',(0.168625710400764,4.17242220359727,-1.28025862071982));
#6497=CARTESIAN_POINT('Ctrl Pts',(0.126469282800573,3.97047197230393,-0.613532492213474));
#6498=CARTESIAN_POINT('Ctrl Pts',(0.0843128552003818,3.76852174101059,0.0531936362928676));
#6499=CARTESIAN_POINT('Ctrl Pts',(0.0421564276001906,3.92881977966068,0.826561622369841));
#6500=CARTESIAN_POINT('Ctrl Pts',(-4.10547488943358E-16,4.38007430561128,
1.36291222925734));
#6501=CARTESIAN_POINT('',(2.73941575321014E-15,7.62290969130025,1.36522594117828));
#6502=CARTESIAN_POINT('Origin',(0.,6.,0.));
#6503=CARTESIAN_POINT('Ctrl Pts',(1.83880688453542E-15,7.62291087731917,
1.36522686078582));
#6504=CARTESIAN_POINT('Ctrl Pts',(0.0412138930502395,7.1828846899475,1.88675593559338));
#6505=CARTESIAN_POINT('Ctrl Pts',(0.0824277861004772,6.4676702007091,2.17777752652732));
#6506=CARTESIAN_POINT('Ctrl Pts',(0.123641679150715,5.78876582874893,2.10968122595389));
#6507=CARTESIAN_POINT('Ctrl Pts',(0.165798106750906,5.09433536159783,2.04002760790171));
#6508=CARTESIAN_POINT('Ctrl Pts',(0.207954534351097,4.4378947790257,1.59464269864839));
#6509=CARTESIAN_POINT('Ctrl Pts',(0.250110961951288,4.11709999477822,0.975083054204924));
#6510=CARTESIAN_POINT('Ctrl Pts',(0.292267389551479,3.79630521053073,0.355523409761457));
#6511=CARTESIAN_POINT('Ctrl Pts',(0.33442381715167,3.81115622460789,-0.438210969872159));
#6512=CARTESIAN_POINT('Ctrl Pts',(0.376580244751861,4.15512217736644,-1.0453657543706));
#6513=CARTESIAN_POINT('Ctrl Pts',(0.418736672352052,4.49908813012499,-1.65252053886904));
#6514=CARTESIAN_POINT('Ctrl Pts',(0.460893099952243,5.17216902156494,-2.07309572823231));
#6515=CARTESIAN_POINT('Ctrl Pts',(0.503049527552434,5.86863390287868,-2.1163069168661));
#6516=CARTESIAN_POINT('Ctrl Pts',(0.545205955152625,6.56509878419243,-2.15951810549988));
#6517=CARTESIAN_POINT('Ctrl Pts',(0.587362382752816,7.28494765537997,-1.82536529340419));
#6518=CARTESIAN_POINT('Ctrl Pts',(0.629518810353007,7.70138276868319,-1.2654790598419));
#6519=CARTESIAN_POINT('Ctrl Pts',(0.656660447227835,7.96949682081299,-0.905006654858185));
#6520=CARTESIAN_POINT('Ctrl Pts',(0.683802084102664,8.11184009736432,-0.450963451734649));
#6521=CARTESIAN_POINT('Ctrl Pts',(0.710943720977492,8.11470858782477,0.00143578057856379));
#6522=CARTESIAN_POINT('Origin',(-1.7667098902285,6.,0.));
#6523=CARTESIAN_POINT('',(10.5667098902285,8.55613055881109,0.000692374991768108));
#6524=CARTESIAN_POINT('',(10.6332901097715,8.56294738394715,-0.00151514723911262));
#6525=CARTESIAN_POINT('',(-1.7667098902285,8.56,1.96795797265743E-13));
#6526=CARTESIAN_POINT('',(11.,3.52700509758159,0.661737268568548));
#6527=CARTESIAN_POINT('Ctrl Pts',(10.6332901097715,8.56294738394715,-0.00151514723911253));
#6528=CARTESIAN_POINT('Ctrl Pts',(10.6712138846473,8.55815224021585,0.75856012002275));
#6529=CARTESIAN_POINT('Ctrl Pts',(10.7512940871233,7.80014953821704,2.37288083670226));
#6530=CARTESIAN_POINT('Ctrl Pts',(10.8735307171994,5.05723750909054,2.86964862298535));
#6531=CARTESIAN_POINT('Ctrl Pts',(10.9578435723998,3.7461035332853,1.48053551427594));
#6532=CARTESIAN_POINT('Ctrl Pts',(11.,3.52700509758159,0.661737268568548));
#6533=CARTESIAN_POINT('',(11.,3.52264482516731,-0.663092573187412));
#6534=CARTESIAN_POINT('Origin',(11.,6.,0.));
#6535=CARTESIAN_POINT('Ctrl Pts',(10.5667098902285,8.55613055881109,0.000692374991768455));
#6536=CARTESIAN_POINT('Ctrl Pts',(10.5856131785684,8.55709447998632,0.382135007947172));
#6537=CARTESIAN_POINT('Ctrl Pts',(10.6466728945084,8.29863237656664,1.61303232131533));
#6538=CARTESIAN_POINT('Ctrl Pts',(10.7498890380487,6.39745114979413,2.99513375481657));
#6539=CARTESIAN_POINT('Ctrl Pts',(10.8754157862993,3.72901154801984,1.97617806422123));
#6540=CARTESIAN_POINT('Ctrl Pts',(10.9587861069498,3.31045923851014,0.134309204987493));
#6541=CARTESIAN_POINT('Ctrl Pts',(11.,3.52264309213417,-0.663093111866542));
#6542=CARTESIAN_POINT('Origin',(-1.7667098902285,6.,0.));
#6543=CARTESIAN_POINT('',(9.76670989022852,8.56017794259811,-0.00227838993089917));
#6544=CARTESIAN_POINT('',(9.8332901097715,8.56018969728858,0.00227386745556037));
#6545=CARTESIAN_POINT('',(-1.7667098902285,8.56,1.96795797265743E-13));
#6546=CARTESIAN_POINT('Ctrl Pts',(9.8332901097715,8.56018969728858,0.00227386745556094));
#6547=CARTESIAN_POINT('Ctrl Pts',(9.84278555811261,8.5619239206668,0.19309848024452));
#6548=CARTESIAN_POINT('Ctrl Pts',(9.89443743405392,8.45560130267874,1.22920413673615));
#6549=CARTESIAN_POINT('Ctrl Pts',(9.98824573759542,7.04679029023846,2.83433283661117));
#6550=CARTESIAN_POINT('Ctrl Pts',(10.114715020396,4.19673876478062,2.42431673808699));
#6551=CARTESIAN_POINT('Ctrl Pts',(10.2411843031966,2.98450817703985,-0.187132765170506));
#6552=CARTESIAN_POINT('Ctrl Pts',(10.3676535859971,4.51025928781023,-2.62891879005706));
#6553=CARTESIAN_POINT('Ctrl Pts',(10.4941228687977,7.38975050690281,-2.68279483089907));
#6554=CARTESIAN_POINT('Ctrl Pts',(10.5826683767225,8.52099523795925,-1.01548145510355));
#6555=CARTESIAN_POINT('Ctrl Pts',(10.6290574570471,8.56348256743679,-0.0863467511938518));
#6556=CARTESIAN_POINT('Ctrl Pts',(10.6332901097715,8.56294738394715,-0.00151514723911253));
#6557=CARTESIAN_POINT('Ctrl Pts',(9.76670989022852,8.56017794259811,-0.00227838993089905));
#6558=CARTESIAN_POINT('Ctrl Pts',(9.79934127963391,8.55422015044893,0.653508106499575));
#6559=CARTESIAN_POINT('Ctrl Pts',(9.8741290966395,7.96469177299003,2.16602528015955));
#6560=CARTESIAN_POINT('Ctrl Pts',(9.99107334124527,5.42536021041376,2.96628144383517));
#6561=CARTESIAN_POINT('Ctrl Pts',(10.1175426240458,3.20108469038192,1.13796721707783));
#6562=CARTESIAN_POINT('Ctrl Pts',(10.2440119068464,3.51849277787554,-1.72375628994429));
#6563=CARTESIAN_POINT('Ctrl Pts',(10.370481189647,6.08955924048204,-3.02010646233692));
#6564=CARTESIAN_POINT('Ctrl Pts',(10.4780471841077,8.20691992499105,-1.7899878009994));
#6565=CARTESIAN_POINT('Ctrl Pts',(10.5434567509682,8.55494482895709,-0.468524329766603));
#6566=CARTESIAN_POINT('Ctrl Pts',(10.5667098902285,8.55613055881109,0.000692374991768455));
#6567=CARTESIAN_POINT('Origin',(-1.7667098902285,6.,0.));
#6568=CARTESIAN_POINT('',(8.96670989022851,8.56310914092999,0.00141529283217118));
#6569=CARTESIAN_POINT('',(9.03329010977151,8.55605974906037,-0.000687443903475848));
#6570=CARTESIAN_POINT('',(-1.7667098902285,8.56,1.96795797265743E-13));
#6571=CARTESIAN_POINT('Ctrl Pts',(9.03329010977151,8.55605974906037,-0.000687443903475485));
#6572=CARTESIAN_POINT('Ctrl Pts',(9.05651365917814,8.55492325759865,0.467936413943757));
#6573=CARTESIAN_POINT('Ctrl Pts',(9.12189363618496,8.20770079733103,1.78879459009414));
#6574=CARTESIAN_POINT('Ctrl Pts',(9.22943004079197,6.09158700182589,3.02003844763038));
#6575=CARTESIAN_POINT('Ctrl Pts',(9.35589932359257,3.51973505278771,1.72548757686079));
#6576=CARTESIAN_POINT('Ctrl Pts',(9.48236860639312,3.20027345136559,-1.1360152149446));
#6577=CARTESIAN_POINT('Ctrl Pts',(9.6088378891937,5.42329849222802,-2.96588214441775));
#6578=CARTESIAN_POINT('Ctrl Pts',(9.72581172365316,7.96382758357787,-2.16718740977869));
#6579=CARTESIAN_POINT('Ctrl Pts',(9.80062913051243,8.55422458308311,-0.654095215554129));
#6580=CARTESIAN_POINT('Ctrl Pts',(9.8332901097715,8.56018969728858,0.00227386745556094));
#6581=CARTESIAN_POINT('Ctrl Pts',(8.96670989022851,8.56310914092999,0.00141529283217119));
#6582=CARTESIAN_POINT('Ctrl Pts',(8.97091295309924,8.56367105037093,0.0856328852446299));
#6583=CARTESIAN_POINT('Ctrl Pts',(9.01727244357015,8.52181940809711,1.01398191393194));
#6584=CARTESIAN_POINT('Ctrl Pts',(9.10578836164127,7.39114764994812,2.68211257580753));
#6585=CARTESIAN_POINT('Ctrl Pts',(9.23225764444183,4.51233920524947,2.62980711778656));
#6586=CARTESIAN_POINT('Ctrl Pts',(9.35872692724241,2.98451046190918,0.189313428699894));
#6587=CARTESIAN_POINT('Ctrl Pts',(9.48519621004298,4.19511541707917,-2.42310002974361));
#6588=CARTESIAN_POINT('Ctrl Pts',(9.61166549284355,7.04478041145962,-2.83504094672479));
#6589=CARTESIAN_POINT('Ctrl Pts',(9.70550338623873,8.4551913903482,-1.2304126453748));
#6590=CARTESIAN_POINT('Ctrl Pts',(9.75718485203372,8.5619170103734,-0.193701174554917));
#6591=CARTESIAN_POINT('Ctrl Pts',(9.76670989022852,8.56017794259811,-0.00227838993089905));
#6592=CARTESIAN_POINT('Origin',(-1.7667098902285,6.,0.));
#6593=CARTESIAN_POINT('',(8.16670989022851,8.55626010879674,0.000990877615878738));
#6594=CARTESIAN_POINT('',(8.23329010977151,8.56264128899482,-0.00167649574357658));
#6595=CARTESIAN_POINT('',(-1.7667098902285,8.56,1.96795797265743E-13));
#6596=CARTESIAN_POINT('Ctrl Pts',(8.23329010977151,8.56264128899483,-0.00167649574357656));
#6597=CARTESIAN_POINT('Ctrl Pts',(8.27024176024366,8.55700984281851,0.739085961748945));
#6598=CARTESIAN_POINT('Ctrl Pts',(8.349349838316,7.83073784367277,2.33458261140701));
#6599=CARTESIAN_POINT('Ctrl Pts',(8.47061434398854,5.12691841598226,2.89253283821776));
#6600=CARTESIAN_POINT('Ctrl Pts',(8.59708362678912,3.09991409354922,0.847655304587422));
#6601=CARTESIAN_POINT('Ctrl Pts',(8.72355290958968,3.70654441823305,-1.96699739921706));
#6602=CARTESIAN_POINT('Ctrl Pts',(8.85002219239026,6.39591418697016,-2.99537475015773));
#6603=CARTESIAN_POINT('Ctrl Pts',(8.9532679257842,8.29791871706444,-1.61424693683209));
#6604=CARTESIAN_POINT('Ctrl Pts',(9.01435723157795,8.55698626782957,-0.382730613268568));
#6605=CARTESIAN_POINT('Ctrl Pts',(9.03329010977151,8.55605974906037,-0.000687443903475485));
#6606=CARTESIAN_POINT('Ctrl Pts',(8.16670989022851,8.55626010879675,0.000990877615879154));
#6607=CARTESIAN_POINT('Ctrl Pts',(8.18464105416476,8.55753072141938,0.362749854559649));
#6608=CARTESIAN_POINT('Ctrl Pts',(8.24472864570121,8.31724292724533,1.57339815673698));
#6609=CARTESIAN_POINT('Ctrl Pts',(8.34697266483782,6.46649534115966,2.98519705577739));
#6610=CARTESIAN_POINT('Ctrl Pts',(8.4734419476384,3.75360435149572,2.02057565464541));
#6611=CARTESIAN_POINT('Ctrl Pts',(8.59991123043897,3.08071680575365,-0.778976857734081));
#6612=CARTESIAN_POINT('Ctrl Pts',(8.72638051323954,5.05889727484518,-2.87112261147709));
#6613=CARTESIAN_POINT('Ctrl Pts',(8.8486467331694,7.79756931010518,-2.37305769290695));
#6614=CARTESIAN_POINT('Ctrl Pts',(8.92875652549905,8.55803513784869,-0.759063695890689));
#6615=CARTESIAN_POINT('Ctrl Pts',(8.96670989022851,8.56310914092999,0.00141529283217119));
#6616=CARTESIAN_POINT('Origin',(-1.7667098902285,6.,0.));
#6617=CARTESIAN_POINT('',(7.36670989022851,8.55959691261755,-0.00228610741251245));
#6618=CARTESIAN_POINT('',(7.4332901097715,8.56078024286682,0.00222060320983035));
#6619=CARTESIAN_POINT('',(-1.7667098902285,8.56,1.96795797265743E-13));
#6620=CARTESIAN_POINT('Ctrl Pts',(7.4332901097715,8.56078024286682,0.00222060320983052));
#6621=CARTESIAN_POINT('Ctrl Pts',(7.44181343370898,8.56233438151834,0.173408601452246));
#6622=CARTESIAN_POINT('Ctrl Pts',(7.49249318524666,8.46889945863842,1.18960690922781));
#6623=CARTESIAN_POINT('Ctrl Pts',(7.58532936438453,7.11139509225075,2.80959402670167));
#6624=CARTESIAN_POINT('Ctrl Pts',(7.71179864718509,4.25280462794925,2.46502048238232));
#6625=CARTESIAN_POINT('Ctrl Pts',(7.83826792998568,2.98088236599169,-0.118094717771357));
#6626=CARTESIAN_POINT('Ctrl Pts',(7.96473721278624,4.45069009732305,-2.59396539404523));
#6627=CARTESIAN_POINT('Ctrl Pts',(8.09120649558682,7.32746169336768,-2.71419658477305));
#6628=CARTESIAN_POINT('Ctrl Pts',(8.18072412791524,8.51042418873668,-1.05464408413909));
#6629=CARTESIAN_POINT('Ctrl Pts',(8.22808533264347,8.56343449909185,-0.10601563748153));
#6630=CARTESIAN_POINT('Ctrl Pts',(8.23329010977151,8.56264128899483,-0.00167649574357656));
#6631=CARTESIAN_POINT('Ctrl Pts',(7.36670989022851,8.55959691261755,-0.00228610741251249));
#6632=CARTESIAN_POINT('Ctrl Pts',(7.39836915523028,8.55391651318035,0.634333487971607));
#6633=CARTESIAN_POINT('Ctrl Pts',(7.47218484783223,7.99282991711364,2.12759389951714));
#6634=CARTESIAN_POINT('Ctrl Pts',(7.58815696803438,5.49345927251859,2.97866343435355));
#6635=CARTESIAN_POINT('Ctrl Pts',(7.71462625083496,3.22786051088117,1.20177452844665));
#6636=CARTESIAN_POINT('Ctrl Pts',(7.84109553363553,3.47970522104534,-1.66647339916602));
#6637=CARTESIAN_POINT('Ctrl Pts',(7.96756481643612,6.02028744265461,-3.02135859893257));
#6638=CARTESIAN_POINT('Ctrl Pts',(8.07610293530042,8.1848475480372,-1.82939795575266));
#6639=CARTESIAN_POINT('Ctrl Pts',(8.14248462656457,8.55454349263577,-0.487750769631392));
#6640=CARTESIAN_POINT('Ctrl Pts',(8.16670989022851,8.55626010879675,0.000990877615879154));
#6641=CARTESIAN_POINT('Origin',(-1.7667098902285,6.,0.));
#6642=CARTESIAN_POINT('',(6.56670989022851,8.5634960952547,0.00112627048192981));
#6643=CARTESIAN_POINT('',(6.6332901097715,8.55593675522896,-0.000379914223101242));
#6644=CARTESIAN_POINT('',(-1.7667098902285,8.56,1.96795797265743E-13));
#6645=CARTESIAN_POINT('Ctrl Pts',(6.6332901097715,8.55593675522896,-0.000379914223101185));
#6646=CARTESIAN_POINT('Ctrl Pts',(6.65554153477451,8.55533662221984,0.448681681498062));
#6647=CARTESIAN_POINT('Ctrl Pts',(6.7199493873777,8.22922127149936,1.74932780794198));
#6648=CARTESIAN_POINT('Ctrl Pts',(6.8265136675811,6.16073061022695,3.01714820944448));
#6649=CARTESIAN_POINT('Ctrl Pts',(6.95298295038165,3.55990612749904,1.78184161478998));
#6650=CARTESIAN_POINT('Ctrl Pts',(7.07945223318224,3.17498687362254,-1.07159623119251));
#6651=CARTESIAN_POINT('Ctrl Pts',(7.2059215159828,5.35552685433585,-2.95189295389255));
#6652=CARTESIAN_POINT('Ctrl Pts',(7.3238674748459,7.93492814248258,-2.20544944201462));
#6653=CARTESIAN_POINT('Ctrl Pts',(7.39965700610879,8.55464759945723,-0.673288591668638));
#6654=CARTESIAN_POINT('Ctrl Pts',(7.4332901097715,8.56078024286682,0.00222060320983052));
#6655=CARTESIAN_POINT('Ctrl Pts',(6.56670989022851,8.5634960952547,0.00112627048193009));
#6656=CARTESIAN_POINT('Ctrl Pts',(6.56994082869561,8.56385434388583,0.065839391593463));
#6657=CARTESIAN_POINT('Ctrl Pts',(6.61532819476289,8.53238654770584,0.974558164011263));
#6658=CARTESIAN_POINT('Ctrl Pts',(6.70287198843037,7.45221141439524,2.64954738997428));
#6659=CARTESIAN_POINT('Ctrl Pts',(6.82934127123096,4.57296049994168,2.66318937161644));
#6660=CARTESIAN_POINT('Ctrl Pts',(6.95581055403151,2.9896368961606,0.258327983142764));
#6661=CARTESIAN_POINT('Ctrl Pts',(7.0822798368321,4.14009309396666,-2.38112697366136));
#6662=CARTESIAN_POINT('Ctrl Pts',(7.20874911963266,6.97957342511075,-2.8582258953101));
#6663=CARTESIAN_POINT('Ctrl Pts',(7.30355913743147,8.44135714864897,-1.27003732301619));
#6664=CARTESIAN_POINT('Ctrl Pts',(7.35621272763009,8.5614803447349,-0.213368057853144));
#6665=CARTESIAN_POINT('Ctrl Pts',(7.36670989022851,8.55959691261755,-0.00228610741251249));
#6666=CARTESIAN_POINT('Origin',(-1.7667098902285,6.,0.));
#6667=CARTESIAN_POINT('',(5.76670989022851,8.55652251069107,0.00126671358662234));
#6668=CARTESIAN_POINT('',(5.83329010977151,8.56213489230814,-0.00188959574180147));
#6669=CARTESIAN_POINT('',(-1.7667098902285,8.56,1.96795797265743E-13));
#6670=CARTESIAN_POINT('Ctrl Pts',(5.8332901097715,8.56213489230814,-0.00188959574180133));
#6671=CARTESIAN_POINT('Ctrl Pts',(5.86926963584003,8.55615869774258,0.719757450352359));
#6672=CARTESIAN_POINT('Ctrl Pts',(5.94740558950873,7.8621596890749,2.29700868724777));
#6673=CARTESIAN_POINT('Ctrl Pts',(6.06769797077765,5.19339550153742,2.91177039443194));
#6674=CARTESIAN_POINT('Ctrl Pts',(6.19416725357823,3.12008881427174,0.913854041489789));
#6675=CARTESIAN_POINT('Ctrl Pts',(6.32063653637879,3.66209554878131,-1.91395413315054));
#6676=CARTESIAN_POINT('Ctrl Pts',(6.44710581917937,6.32720695415856,-3.00365664748478));
#6677=CARTESIAN_POINT('Ctrl Pts',(6.55132367697694,8.27854620458815,-1.653862511724));
#6678=CARTESIAN_POINT('Ctrl Pts',(6.61338510717432,8.5564736039523,-0.402087770143315));
#6679=CARTESIAN_POINT('Ctrl Pts',(6.6332901097715,8.55593675522896,-0.000379914223101185));
#6680=CARTESIAN_POINT('Ctrl Pts',(5.76670989022851,8.55652251069107,0.00126671358662286));
#6681=CARTESIAN_POINT('Ctrl Pts',(5.78366892976113,8.55806819340342,0.343325249083328));
#6682=CARTESIAN_POINT('Ctrl Pts',(5.84278439689394,8.33538619924687,1.53373602056116));
#6683=CARTESIAN_POINT('Ctrl Pts',(5.94405629162693,6.53474335439746,2.97372979753514));
#6684=CARTESIAN_POINT('Ctrl Pts',(6.07052557442751,3.80047113580028,2.07149514587238));
#6685=CARTESIAN_POINT('Ctrl Pts',(6.19699485722809,3.06364154273657,-0.711911774223792));
#6686=CARTESIAN_POINT('Ctrl Pts',(6.32346414002865,4.99338643380372,-2.84881527870274));
#6687=CARTESIAN_POINT('Ctrl Pts',(6.44670248436214,7.76460713319277,-2.41014488541846));
#6688=CARTESIAN_POINT('Ctrl Pts',(6.52778440109542,8.55918001082909,-0.778520237258299));
#6689=CARTESIAN_POINT('Ctrl Pts',(6.56670989022851,8.5634960952547,0.00112627048193009));
#6690=CARTESIAN_POINT('Origin',(-1.7667098902285,6.,0.));
#6691=CARTESIAN_POINT('',(4.96670989022851,8.55903014885295,-0.00224703052746647));
#6692=CARTESIAN_POINT('',(5.0332901097715,8.56135690444116,0.00211620437658548));
#6693=CARTESIAN_POINT('',(-1.7667098902285,8.56,1.96795797265743E-13));
#6694=CARTESIAN_POINT('Ctrl Pts',(5.0332901097715,8.56135690444116,0.00211620437658528));
#6695=CARTESIAN_POINT('Ctrl Pts',(5.04084130930536,8.56270384795118,0.153691292555975));
#6696=CARTESIAN_POINT('Ctrl Pts',(5.0905489364394,8.48167485146914,1.15003395919758));
#6697=CARTESIAN_POINT('Ctrl Pts',(5.18241299117364,7.17545208301331,2.78340260245806));
#6698=CARTESIAN_POINT('Ctrl Pts',(5.30888227397421,4.30971964307301,2.50439013770165));
#6699=CARTESIAN_POINT('Ctrl Pts',(5.43535155677478,2.97896957548569,-0.0489164695102037));
#6700=CARTESIAN_POINT('Ctrl Pts',(5.56182083957536,4.39168654812479,-2.55780090846567));
#6701=CARTESIAN_POINT('Ctrl Pts',(5.68829012237593,7.26494986606656,-2.74388765862757));
#6702=CARTESIAN_POINT('Ctrl Pts',(5.77877987910798,8.49886688840039,-1.0941409336459));
#6703=CARTESIAN_POINT('Ctrl Pts',(5.82711320823984,8.56316087484319,-0.125780686909922));
#6704=CARTESIAN_POINT('Ctrl Pts',(5.8332901097715,8.56213489230814,-0.00188959574180133));
#6705=CARTESIAN_POINT('Ctrl Pts',(4.96670989022851,8.55903014885295,-0.00224703052746637));
#6706=CARTESIAN_POINT('Ctrl Pts',(4.99739703082665,8.55371858466909,0.615172981798587));
#6707=CARTESIAN_POINT('Ctrl Pts',(5.07024059902498,8.02025392240756,2.08900571630608));
#6708=CARTESIAN_POINT('Ctrl Pts',(5.18524059482349,5.56181288602103,2.98948346992642));
#6709=CARTESIAN_POINT('Ctrl Pts',(5.31170987762408,3.2561120833366,1.26494998502281));
#6710=CARTESIAN_POINT('Ctrl Pts',(5.43817916042463,3.44219885099807,-1.60831360312132));
#6711=CARTESIAN_POINT('Ctrl Pts',(5.56464844322522,5.9510835258896,-3.02103070861275));
#6712=CARTESIAN_POINT('Ctrl Pts',(5.67415868649317,8.16200184373334,-1.86872894720649));
#6713=CARTESIAN_POINT('Ctrl Pts',(5.74151250216094,8.55422596747839,-0.506956741176808));
#6714=CARTESIAN_POINT('Ctrl Pts',(5.76670989022851,8.55652251069107,0.00126671358662286));
#6715=CARTESIAN_POINT('Origin',(-1.7667098902285,6.,0.));
#6716=CARTESIAN_POINT('',(4.16670989022851,8.56380264418621,0.000808262703818619));
#6717=CARTESIAN_POINT('',(4.2332901097715,8.55588550426825,-6.54012209720356E-5));
#6718=CARTESIAN_POINT('',(-1.7667098902285,8.56,1.96795797265743E-13));
#6719=CARTESIAN_POINT('Ctrl Pts',(4.2332901097715,8.55588550426825,-6.54012209719279E-5));
#6720=CARTESIAN_POINT('Ctrl Pts',(4.25456941037088,8.55578681917127,0.429399022051573));
#6721=CARTESIAN_POINT('Ctrl Pts',(4.31800513857044,8.2501018113131,1.70980750910722));
#6722=CARTESIAN_POINT('Ctrl Pts',(4.42359729437019,6.22979061312465,3.01267554193145));
#6723=CARTESIAN_POINT('Ctrl Pts',(4.55006657717078,3.60135595755754,1.83726002636678));
#6724=CARTESIAN_POINT('Ctrl Pts',(4.67653585997134,3.1511849892005,-1.00661347153406));
#6725=CARTESIAN_POINT('Ctrl Pts',(4.80300514277192,5.28808829272449,-2.93635818112757));
#6726=CARTESIAN_POINT('Ctrl Pts',(4.92192322603863,7.90530393143438,-2.24352310907718));
#6727=CARTESIAN_POINT('Ctrl Pts',(4.99868488170516,8.55518420470679,-0.692513896722687));
#6728=CARTESIAN_POINT('Ctrl Pts',(5.0332901097715,8.56135690444116,0.00211620437658528));
#6729=CARTESIAN_POINT('Ctrl Pts',(4.16670989022851,8.56380264418621,0.000808262703819061));
#6730=CARTESIAN_POINT('Ctrl Pts',(4.16896870429198,8.56399082802434,0.0460361249824619));
#6731=CARTESIAN_POINT('Ctrl Pts',(4.21338394595564,8.54247712043068,0.935172573537014));
#6732=CARTESIAN_POINT('Ctrl Pts',(4.29995561521948,7.51251343469132,2.61559218413545));
#6733=CARTESIAN_POINT('Ctrl Pts',(4.42642489802006,4.63433022445025,2.69517447078429));
#6734=CARTESIAN_POINT('Ctrl Pts',(4.55289418082063,2.99634307005063,0.327206984929225));
#6735=CARTESIAN_POINT('Ctrl Pts',(4.6793634636212,4.08604568686072,-2.33790467107576));
#6736=CARTESIAN_POINT('Ctrl Pts',(4.80583274642178,6.91385412742878,-2.87991145655582));
#6737=CARTESIAN_POINT('Ctrl Pts',(4.90161488862421,8.4269861859368,-1.30968214690492));
#6738=CARTESIAN_POINT('Ctrl Pts',(4.95524060322645,8.56101534046309,-0.23300712039416));
#6739=CARTESIAN_POINT('Ctrl Pts',(4.96670989022851,8.55903014885295,-0.00224703052746637));
#6740=CARTESIAN_POINT('Origin',(-1.7667098902285,6.,0.));
#6741=CARTESIAN_POINT('',(3.36670989022851,8.55684831657772,0.00151882186684854));
#6742=CARTESIAN_POINT('',(3.4332901097715,8.56159030865862,-0.00205930216014198));
#6743=CARTESIAN_POINT('',(-1.7667098902285,8.56,1.96795797265743E-13));
#6744=CARTESIAN_POINT('Ctrl Pts',(3.4332901097715,8.56159030865862,-0.00205930216014198));
#6745=CARTESIAN_POINT('Ctrl Pts',(3.46829751143639,8.55544255054036,0.700477784773422));
#6746=CARTESIAN_POINT('Ctrl Pts',(3.54546134070149,7.89283216702593,2.25921760989519));
#6747=CARTESIAN_POINT('Ctrl Pts',(3.66478159756676,5.26029576462132,2.92948037902181));
#6748=CARTESIAN_POINT('Ctrl Pts',(3.79125088036734,3.14177437347817,0.979573332991449));
#6749=CARTESIAN_POINT('Ctrl Pts',(3.9177201631679,3.61887325026032,-1.85990673112716));
#6750=CARTESIAN_POINT('Ctrl Pts',(4.04418944596849,6.25832795884948,-3.01036282074418));
#6751=CARTESIAN_POINT('Ctrl Pts',(4.14937942816968,8.2585551860386,-1.69344410064111));
#6752=CARTESIAN_POINT('Ctrl Pts',(4.21241298277068,8.55598232424093,-0.421413051493609));
#6753=CARTESIAN_POINT('Ctrl Pts',(4.2332901097715,8.55588550426825,-6.54012209719279E-5));
#6754=CARTESIAN_POINT('Ctrl Pts',(3.36670989022851,8.55684831657772,0.00151882186684858));
#6755=CARTESIAN_POINT('Ctrl Pts',(3.3826968053575,8.55860910445953,0.323866842439612));
#6756=CARTESIAN_POINT('Ctrl Pts',(3.44084014808668,8.3529374416759,1.49406099706874));
#6757=CARTESIAN_POINT('Ctrl Pts',(3.54113991841604,6.60271083165986,2.96070245343145));
#6758=CARTESIAN_POINT('Ctrl Pts',(3.66760920121663,3.84849183796069,2.12132788423443));
#6759=CARTESIAN_POINT('Ctrl Pts',(3.79407848401719,3.0481067685106,-0.644473206270731));
#6760=CARTESIAN_POINT('Ctrl Pts',(3.92054776681777,4.92840366803431,-2.82501339204223));
#6761=CARTESIAN_POINT('Ctrl Pts',(4.04475823555487,7.73087773797067,-2.44696898167379));
#6762=CARTESIAN_POINT('Ctrl Pts',(4.12681227669178,8.56047873799623,-0.79805508752461));
#6763=CARTESIAN_POINT('Ctrl Pts',(4.16670989022851,8.56380264418621,0.000808262703819061));
#6764=CARTESIAN_POINT('Origin',(-1.7667098902285,6.,0.));
#6765=CARTESIAN_POINT('',(2.56670989022851,8.55848755255065,-0.00216282574899321));
#6766=CARTESIAN_POINT('',(2.6332901097715,8.56191347466111,0.00196523236974941));
#6767=CARTESIAN_POINT('',(-1.7667098902285,8.56,1.96795797265743E-13));
#6768=CARTESIAN_POINT('Ctrl Pts',(2.6332901097715,8.56191347466111,0.00196523236974947));
#6769=CARTESIAN_POINT('Ctrl Pts',(2.63986918490172,8.56303541238676,0.133952476013648));
#6770=CARTESIAN_POINT('Ctrl Pts',(2.68860468763214,8.49394004679471,1.11049084410191));
#6771=CARTESIAN_POINT('Ctrl Pts',(2.77949661796275,7.23889240500353,2.75575094100713));
#6772=CARTESIAN_POINT('Ctrl Pts',(2.90596590076332,4.36752141768572,2.5424459342591));
#6773=CARTESIAN_POINT('Ctrl Pts',(3.0324351835639,2.97864168519721,0.0202874407439004));
#6774=CARTESIAN_POINT('Ctrl Pts',(3.15890446636446,4.33352675754921,-2.52029454194393));
#6775=CARTESIAN_POINT('Ctrl Pts',(3.28537374916504,7.20177441543159,-2.77213922842707));
#6776=CARTESIAN_POINT('Ctrl Pts',(3.37683563030072,8.48681045755432,-1.13367097303057));
#6777=CARTESIAN_POINT('Ctrl Pts',(3.4261410838362,8.562845771222,-0.145527700731133));
#6778=CARTESIAN_POINT('Ctrl Pts',(3.4332901097715,8.56159030865862,-0.00205930216014198));
#6779=CARTESIAN_POINT('Ctrl Pts',(2.56670989022851,8.55848755255065,-0.00216282574899286));
#6780=CARTESIAN_POINT('Ctrl Pts',(2.59642490642302,8.55361826490113,0.596020238525012));
#6781=CARTESIAN_POINT('Ctrl Pts',(2.66829635021771,8.04696672892027,2.05027352543945));
#6782=CARTESIAN_POINT('Ctrl Pts',(2.78232422161261,5.63039638482652,2.99873515893208));
#6783=CARTESIAN_POINT('Ctrl Pts',(2.90879350441318,3.28580315999094,1.32746181821946));
#6784=CARTESIAN_POINT('Ctrl Pts',(3.03526278721375,3.4060343620134,-1.54931004838359));
#6785=CARTESIAN_POINT('Ctrl Pts',(3.16173207001433,5.88190527112525,-3.01911791792189));
#6786=CARTESIAN_POINT('Ctrl Pts',(3.27221443768591,8.13849045765698,-1.90797857169019));
#6787=CARTESIAN_POINT('Ctrl Pts',(3.34054037775731,8.55396602439938,-0.526143361636563));
#6788=CARTESIAN_POINT('Ctrl Pts',(3.36670989022851,8.55684831657772,0.00151882186684858));
#6789=CARTESIAN_POINT('Origin',(-1.7667098902285,6.,0.));
#6790=CARTESIAN_POINT('',(1.76670989022851,8.56401420494256,0.000468657028373232));
#6791=CARTESIAN_POINT('',(1.8332901097715,8.55590678256854,0.000250277143156217));
#6792=CARTESIAN_POINT('',(-1.7667098902285,8.56,1.96795797265743E-13));
#6793=CARTESIAN_POINT('Ctrl Pts',(1.8332901097715,8.55590678256854,0.000250277143156244));
#6794=CARTESIAN_POINT('Ctrl Pts',(1.85359728596724,8.55626740670647,0.410086533789295));
#6795=CARTESIAN_POINT('Ctrl Pts',(1.91606088976318,8.27035132529504,1.67024228262478));
#6796=CARTESIAN_POINT('Ctrl Pts',(2.02068092115931,6.29873006674212,3.00662229441761));
#6797=CARTESIAN_POINT('Ctrl Pts',(2.14715020395988,3.6440641683139,1.89171460246179));
#6798=CARTESIAN_POINT('Ctrl Pts',(2.27361948676046,3.12887765854667,-0.941102636765302));
#6799=CARTESIAN_POINT('Ctrl Pts',(2.40008876956103,5.221023215509,-2.91928291965494));
#6800=CARTESIAN_POINT('Ctrl Pts',(2.51997897723137,7.87493959029486,-2.28139980516642));
#6801=CARTESIAN_POINT('Ctrl Pts',(2.59771275730153,8.55584642524694,-0.711775923599712));
#6802=CARTESIAN_POINT('Ctrl Pts',(2.6332901097715,8.56191347466111,0.00196523236974947));
#6803=CARTESIAN_POINT('Ctrl Pts',(1.76670989022851,8.56401420494256,0.000468657028373227));
#6804=CARTESIAN_POINT('Ctrl Pts',(1.76799657988834,8.56407959778106,0.0262261544125052));
#6805=CARTESIAN_POINT('Ctrl Pts',(1.81143969714837,8.55209842073233,0.895826509796029));
#6806=CARTESIAN_POINT('Ctrl Pts',(1.89703924200859,7.57202172994746,2.58026440683785));
#6807=CARTESIAN_POINT('Ctrl Pts',(2.02350852480917,4.69641652838636,2.72574581528328));
#6808=CARTESIAN_POINT('Ctrl Pts',(2.14997780760974,3.00462496841716,0.395914224840739));
#6809=CARTESIAN_POINT('Ctrl Pts',(2.27644709041032,4.03300241565958,-2.29345579779455));
#6810=CARTESIAN_POINT('Ctrl Pts',(2.40291637321088,6.8476553843829,-2.90008617898366));
#6811=CARTESIAN_POINT('Ctrl Pts',(2.49967063981696,8.41207197849935,-1.34934333695958));
#6812=CARTESIAN_POINT('Ctrl Pts',(2.55426847882283,8.56052627972158,-0.252616722520519));
#6813=CARTESIAN_POINT('Ctrl Pts',(2.56670989022851,8.55848755255065,-0.00216282574899286));
#6814=CARTESIAN_POINT('Origin',(-1.7667098902285,6.,0.));
#6815=CARTESIAN_POINT('',(0.966709890228505,8.55722909061475,0.00173622970309428));
#6816=CARTESIAN_POINT('',(1.0332901097715,8.5610206941956,-0.00218674593362891));
#6817=CARTESIAN_POINT('',(-1.7667098902285,8.56,1.96795797265743E-13));
#6818=CARTESIAN_POINT('Ctrl Pts',(1.0332901097715,8.5610206941956,-0.00218674593362883));
#6819=CARTESIAN_POINT('Ctrl Pts',(1.06732538703276,8.55485502342069,0.681234786359444));
#6820=CARTESIAN_POINT('Ctrl Pts',(1.14351709189422,7.92276141437229,2.22122903234413));
#6821=CARTESIAN_POINT('Ctrl Pts',(1.26186522435587,5.32758429305789,2.94565042609802));
#6822=CARTESIAN_POINT('Ctrl Pts',(1.38833450715645,3.16495931797173,1.0447803202184));
#6823=CARTESIAN_POINT('Ctrl Pts',(1.51480378995702,3.57690019914092,-1.80488441711536));
#6824=CARTESIAN_POINT('Ctrl Pts',(1.64127307275759,6.18931341035722,-3.01548925232429));
#6825=CARTESIAN_POINT('Ctrl Pts',(1.74743517936242,8.23793676912792,-1.73298413552372));
#6826=CARTESIAN_POINT('Ctrl Pts',(1.81144085836705,8.5555187735526,-0.440707900389815));
#6827=CARTESIAN_POINT('Ctrl Pts',(1.8332901097715,8.55590678256854,0.000250277143156244));
#6828=CARTESIAN_POINT('Ctrl Pts',(0.966709890228505,8.55722909061475,0.00173622970309435));
#6829=CARTESIAN_POINT('Ctrl Pts',(0.981724680953864,8.55914800573449,0.304374756490232));
#6830=CARTESIAN_POINT('Ctrl Pts',(1.03889589927941,8.36991977797047,1.45440284520618));
#6831=CARTESIAN_POINT('Ctrl Pts',(1.13822354520516,6.67035096999308,2.94610350710691));
#6832=CARTESIAN_POINT('Ctrl Pts',(1.26469282800573,3.89764709051462,2.17005731163833));
#6833=CARTESIAN_POINT('Ctrl Pts',(1.39116211080631,3.0341175837159,-0.576701540113256));
#6834=CARTESIAN_POINT('Ctrl Pts',(1.51763139360688,4.8639846740404,-2.79972682418719));
#6835=CARTESIAN_POINT('Ctrl Pts',(1.64281398674761,7.69637500900364,-2.48351535416102));
#6836=CARTESIAN_POINT('Ctrl Pts',(1.72584015228815,8.56193710099446,-0.817679029197883));
#6837=CARTESIAN_POINT('Ctrl Pts',(1.76670989022851,8.56401420494256,0.000468657028373227));
#6838=CARTESIAN_POINT('Origin',(-1.7667098902285,6.,0.));
#6839=CARTESIAN_POINT('',(0.166709890228505,8.55738198002468,-0.00304066224802793));
#6840=CARTESIAN_POINT('',(0.233290109771496,8.56244188004781,0.00169655094858915));
#6841=CARTESIAN_POINT('',(-1.7667098902285,8.56,1.96795797265743E-13));
#6842=CARTESIAN_POINT('',(0.,6.66173726856851,-2.47299490241842));
#6843=CARTESIAN_POINT('Ctrl Pts',(0.,6.66173726856851,-2.47299490241842));
#6844=CARTESIAN_POINT('Ctrl Pts',(0.042156427600191,7.4805355142759,-2.25389646671472));
#6845=CARTESIAN_POINT('Ctrl Pts',(0.0977263910096926,8.39608892768013,-1.38973499298135));
#6846=CARTESIAN_POINT('Ctrl Pts',(0.153296354419194,8.55936199509083,-0.273279593862165));
#6847=CARTESIAN_POINT('Ctrl Pts',(0.166709890228505,8.55738198002468,-0.00304066224802793));
#6848=CARTESIAN_POINT('',(1.04028710533623E-16,5.33690806430729,-2.47735557113815));
#6849=CARTESIAN_POINT('Origin',(0.,6.,0.));
#6850=CARTESIAN_POINT('Ctrl Pts',(-1.76182853028894E-18,5.33690753016716,
-2.47735729053333));
#6851=CARTESIAN_POINT('Ctrl Pts',(0.0412138930502383,6.13431011265186,-2.68954137333078));
#6852=CARTESIAN_POINT('Ctrl Pts',(0.11897726297407,7.85230474856696,-2.29913620624405));
#6853=CARTESIAN_POINT('Ctrl Pts',(0.196740632897902,8.55663316562353,-0.730968810525245));
#6854=CARTESIAN_POINT('Ctrl Pts',(0.233290109771496,8.56244188004781,0.00169655094858908));
#6855=CARTESIAN_POINT('Origin',(2.5,0.,-3.));
#6856=CARTESIAN_POINT('',(0.,1.,-3.));
#6857=CARTESIAN_POINT('Origin',(0.,0.,-3.));
#6858=CARTESIAN_POINT('',(5.,1.,-3.));
#6859=CARTESIAN_POINT('',(2.5,1.,-3.));
#6860=CARTESIAN_POINT('Origin',(5.,0.,-3.));
#6861=CARTESIAN_POINT('Origin',(5.,0.,-3.));
#6862=CARTESIAN_POINT('Origin',(2.5,0.,3.));
#6863=CARTESIAN_POINT('',(0.,1.,3.));
#6864=CARTESIAN_POINT('Origin',(0.,0.,3.));
#6865=CARTESIAN_POINT('',(5.,1.,3.));
#6866=CARTESIAN_POINT('',(2.5,1.,3.));
#6867=CARTESIAN_POINT('Origin',(5.,0.,3.));
#6868=CARTESIAN_POINT('Origin',(5.,0.,3.));
#6869=CARTESIAN_POINT('Origin',(11.,6.,0.));
#6870=CARTESIAN_POINT('Ctrl Pts',(11.,7.36291222925731,-1.61992569438875));
#6871=CARTESIAN_POINT('Ctrl Pts',(11.,7.31083931682775,-1.67389112219309));
#6872=CARTESIAN_POINT('Ctrl Pts',(11.,7.25581777272501,-1.72471964452079));
#6873=CARTESIAN_POINT('Ctrl Pts',(11.,7.19820656866207,-1.77240154562655));
#6874=CARTESIAN_POINT('Ctrl Pts',(11.,7.13906939943468,-1.82134641148449));
#6875=CARTESIAN_POINT('Ctrl Pts',(11.,7.07720303473932,-1.86697624806703));
#6876=CARTESIAN_POINT('Ctrl Pts',(11.,7.0129505096539,-1.90924986985927));
#6877=CARTESIAN_POINT('Ctrl Pts',(11.,6.99905883361936,-1.91838961118404));
#6878=CARTESIAN_POINT('Ctrl Pts',(11.,6.98505362557214,-1.92737349175926));
#6879=CARTESIAN_POINT('Ctrl Pts',(11.,6.97094405837831,-1.93619717947497));
#6880=CARTESIAN_POINT('Ctrl Pts',(11.,6.90417313060292,-1.97795365627432));
#6881=CARTESIAN_POINT('Ctrl Pts',(11.,6.83519118466879,-2.01605003484858));
#6882=CARTESIAN_POINT('Ctrl Pts',(11.,6.76437461164589,-2.05045793329471));
#6883=CARTESIAN_POINT('Ctrl Pts',(11.,6.70878554997294,-2.07746718702039));
#6884=CARTESIAN_POINT('Ctrl Pts',(11.,6.65206493296289,-2.10220311337323));
#6885=CARTESIAN_POINT('Ctrl Pts',(11.,6.59437882701511,-2.12463622451561));
#6886=CARTESIAN_POINT('Ctrl Pts',(11.,6.57496243421673,-2.13218691788403));
#6887=CARTESIAN_POINT('Ctrl Pts',(11.,6.55543656169613,-2.13947659865928));
#6888=CARTESIAN_POINT('Ctrl Pts',(11.,6.53580726721147,-2.14650375048553));
#6889=CARTESIAN_POINT('Ctrl Pts',(11.,6.51922223942772,-2.15244107586267));
#6890=CARTESIAN_POINT('Ctrl Pts',(11.,6.5025612632835,-2.15819155491499));
#6891=CARTESIAN_POINT('Ctrl Pts',(11.,6.48585004814776,-2.16374720263022));
#6892=CARTESIAN_POINT('Ctrl Pts',(11.,6.40908866330734,-2.18926654451187));
#6893=CARTESIAN_POINT('Ctrl Pts',(11.,6.33117162879884,-2.21071471076539));
#6894=CARTESIAN_POINT('Ctrl Pts',(11.,6.25247824483006,-2.22806194232001));
#6895=CARTESIAN_POINT('Ctrl Pts',(11.,6.17264608791968,-2.24566020587898));
#6896=CARTESIAN_POINT('Ctrl Pts',(11.,6.09201408999904,-2.25903848278578));
#6897=CARTESIAN_POINT('Ctrl Pts',(11.,6.0109467640778,-2.26812293923578));
#6898=CARTESIAN_POINT('Ctrl Pts',(11.,5.93065938032486,-2.277119994867));
#6899=CARTESIAN_POINT('Ctrl Pts',(11.,5.84994403510389,-2.28190578244251));
#6900=CARTESIAN_POINT('Ctrl Pts',(11.,5.76913803616273,-2.28236102601123));
#6901=CARTESIAN_POINT('Ctrl Pts',(11.,5.73623455271216,-2.28254639713993));
#6902=CARTESIAN_POINT('Ctrl Pts',(11.,5.70331592490547,-2.28201316467977));
#6903=CARTESIAN_POINT('Ctrl Pts',(11.,5.67040468508686,-2.28075078754997));
#6904=CARTESIAN_POINT('Ctrl Pts',(11.,5.65686480751649,-2.28023143817633));
#6905=CARTESIAN_POINT('Ctrl Pts',(11.,5.64332427555182,-2.27958848039974));
#6906=CARTESIAN_POINT('Ctrl Pts',(11.,5.62980206611338,-2.27882230599476));
#6907=CARTESIAN_POINT('Ctrl Pts',(11.,5.54615795497388,-2.27408299343094));
#6908=CARTESIAN_POINT('Ctrl Pts',(11.,5.46307785440037,-2.26462914348589));
#6909=CARTESIAN_POINT('Ctrl Pts',(11.,5.38093981928942,-2.25039680394637));
#6910=CARTESIAN_POINT('Ctrl Pts',(11.,5.36156670336747,-2.24703995759173));
#6911=CARTESIAN_POINT('Ctrl Pts',(11.,5.34224591428098,-2.24341706956682));
#6912=CARTESIAN_POINT('Ctrl Pts',(11.,5.32298228814404,-2.23952689585244));
#6913=CARTESIAN_POINT('Ctrl Pts',(11.,5.24431074388793,-2.22363964952824));
#6914=CARTESIAN_POINT('Ctrl Pts',(11.,5.1665925882148,-2.2032986905466));
#6915=CARTESIAN_POINT('Ctrl Pts',(11.,5.0900490421026,-2.1787929080781));
#6916=CARTESIAN_POINT('Ctrl Pts',(11.,5.01174129876329,-2.1537223094275));
#6917=CARTESIAN_POINT('Ctrl Pts',(11.,4.93466218929701,-2.12429244228821));
#6918=CARTESIAN_POINT('Ctrl Pts',(11.,4.85905468736252,-2.09075876968975));
#6919=CARTESIAN_POINT('Ctrl Pts',(11.,4.84209216260409,-2.08323549835901));
#6920=CARTESIAN_POINT('Ctrl Pts',(11.,4.82520375806804,-2.07550546979706));
#6921=CARTESIAN_POINT('Ctrl Pts',(11.,4.80839231975368,-2.06757122910378));
#6922=CARTESIAN_POINT('Ctrl Pts',(11.,4.79129520538481,-2.05950216219669));
#6923=CARTESIAN_POINT('Ctrl Pts',(11.,4.77427243502448,-2.05121911042241));
#6924=CARTESIAN_POINT('Ctrl Pts',(11.,4.7573567617439,-2.04273992899805));
#6925=CARTESIAN_POINT('Ctrl Pts',(11.,4.68205610488726,-2.00499458358553));
#6926=CARTESIAN_POINT('Ctrl Pts',(11.,4.60878482621383,-1.96332639890493));
#6927=CARTESIAN_POINT('Ctrl Pts',(11.,4.53777905821884,-1.91806485765549));
#6928=CARTESIAN_POINT('Ctrl Pts',(11.,4.46532239493622,-1.87187846538671));
#6929=CARTESIAN_POINT('Ctrl Pts',(11.,4.39522396629416,-1.82195001563772));
#6930=CARTESIAN_POINT('Ctrl Pts',(11.,4.32774333179297,-1.76857493043294));
#6931=CARTESIAN_POINT('Ctrl Pts',(11.,4.25977928024263,-1.71481747736249));
#6932=CARTESIAN_POINT('Ctrl Pts',(11.,4.19446979653655,-1.65756332034335));
#6933=CARTESIAN_POINT('Ctrl Pts',(11.,4.13210143705822,-1.59706609202154));
#6934=CARTESIAN_POINT('Ctrl Pts',(11.,4.11241075428857,-1.57796615510975));
#6935=CARTESIAN_POINT('Ctrl Pts',(11.,4.09301344480314,-1.55854263321621));
#6936=CARTESIAN_POINT('Ctrl Pts',(11.,4.07391918281171,-1.53880264867837));
#6937=CARTESIAN_POINT('Ctrl Pts',(11.,4.06113823260671,-1.5255894771225));
#6938=CARTESIAN_POINT('Ctrl Pts',(11.,4.04849306806107,-1.51223450831911));
#6939=CARTESIAN_POINT('Ctrl Pts',(11.,4.03598668555857,-1.49873978569596));
#6940=CARTESIAN_POINT('Ctrl Pts',(11.,4.02703668266137,-1.48908249218603));
#6941=CARTESIAN_POINT('Ctrl Pts',(11.,4.01815874529529,-1.47935459918655));
#6942=CARTESIAN_POINT('Ctrl Pts',(11.,4.00936203992878,-1.46956616048432));
#6943=CARTESIAN_POINT('Ctrl Pts',(11.,3.94979319594867,-1.40328157397517));
#6944=CARTESIAN_POINT('Ctrl Pts',(11.,3.89384398506478,-1.33411346169234));
#6945=CARTESIAN_POINT('Ctrl Pts',(11.,3.84178206189435,-1.26237691191309));
#6946=CARTESIAN_POINT('Ctrl Pts',(11.,3.7896896723596,-1.19059838228127));
#6947=CARTESIAN_POINT('Ctrl Pts',(11.,3.74148825905101,-1.11624778861253));
#6948=CARTESIAN_POINT('Ctrl Pts',(11.,3.69747310618552,-1.03959646371966));
#6949=CARTESIAN_POINT('Ctrl Pts',(11.,3.65443166340002,-0.964640831397038));
#6950=CARTESIAN_POINT('Ctrl Pts',(11.,3.61539263220366,-0.887484432473658));
#6951=CARTESIAN_POINT('Ctrl Pts',(11.,3.58066926892089,-0.808348627556223));
#6952=CARTESIAN_POINT('Ctrl Pts',(11.,3.56732500935102,-0.777936575777442));
#6953=CARTESIAN_POINT('Ctrl Pts',(11.,3.55461857152964,-0.747231898960612));
#6954=CARTESIAN_POINT('Ctrl Pts',(11.,3.54256956733971,-0.716246178019685));
#6955=CARTESIAN_POINT('Ctrl Pts',(11.,3.53571486427718,-0.698618338168349));
#6956=CARTESIAN_POINT('Ctrl Pts',(11.,3.52907296049142,-0.680899529254575));
#6957=CARTESIAN_POINT('Ctrl Pts',(11.,3.52264309213416,-0.663093111866506));
#6958=CARTESIAN_POINT('Ctrl Pts',(11.,3.52700509758159,0.661737268568549));
#6959=CARTESIAN_POINT('Ctrl Pts',(11.,3.55700783839337,0.744600185400307));
#6960=CARTESIAN_POINT('Ctrl Pts',(11.,3.59157342721284,0.825613106651542));
#6961=CARTESIAN_POINT('Ctrl Pts',(11.,3.63039754344568,0.904544394731748));
#6962=CARTESIAN_POINT('Ctrl Pts',(11.,3.67052378457075,0.9861229650931));
#6963=CARTESIAN_POINT('Ctrl Pts',(11.,3.71519964166936,1.06547878949095));
#6964=CARTESIAN_POINT('Ctrl Pts',(11.,3.76413235433514,1.14231972468823));
#6965=CARTESIAN_POINT('Ctrl Pts',(11.,3.77380220479441,1.1575046656414));
#6966=CARTESIAN_POINT('Ctrl Pts',(11.,3.78363840594323,1.17259126130582));
#6967=CARTESIAN_POINT('Ctrl Pts',(11.,3.79363885408994,1.18757704999784));
#6968=CARTESIAN_POINT('Ctrl Pts',(11.,3.80363720316686,1.20255969320921));
#6969=CARTESIAN_POINT('Ctrl Pts',(11.,3.81379421168505,1.21743327691453));
#6970=CARTESIAN_POINT('Ctrl Pts',(11.,3.8241061116684,1.23219400682824));
#6971=CARTESIAN_POINT('Ctrl Pts',(11.,3.87459514587875,1.30446536310462));
#6972=CARTESIAN_POINT('Ctrl Pts',(11.,3.92880390516673,1.37404842935174));
#6973=CARTESIAN_POINT('Ctrl Pts',(11.,3.98645173205705,1.44068424654798));
#6974=CARTESIAN_POINT('Ctrl Pts',(11.,4.02844581867207,1.48922571688519));
#6975=CARTESIAN_POINT('Ctrl Pts',(11.,4.07226572854448,1.5362025213652));
#6976=CARTESIAN_POINT('Ctrl Pts',(11.,4.11781249583983,1.58149996077335));
#6977=CARTESIAN_POINT('Ctrl Pts',(11.,4.13416564266894,1.59776358872352));
#6978=CARTESIAN_POINT('Ctrl Pts',(11.,4.15074145945183,1.61381060316234));
#6979=CARTESIAN_POINT('Ctrl Pts',(11.,4.16753554575574,1.62963525480062));
#6980=CARTESIAN_POINT('Ctrl Pts',(11.,4.17867242794955,1.64012926309999));
#6981=CARTESIAN_POINT('Ctrl Pts',(11.,4.18989915573443,1.65051965601333));
#6982=CARTESIAN_POINT('Ctrl Pts',(11.,4.20121078938897,1.66080208045739));
#6983=CARTESIAN_POINT('Ctrl Pts',(11.,4.26495358312366,1.71874512214768));
#6984=CARTESIAN_POINT('Ctrl Pts',(11.,4.33142426322727,1.77329526969942));
#6985=CARTESIAN_POINT('Ctrl Pts',(11.,4.40035782940769,1.82421550306439));
#6986=CARTESIAN_POINT('Ctrl Pts',(11.,4.46792796306447,1.87412858844431));
#6987=CARTESIAN_POINT('Ctrl Pts',(11.,4.53786533886277,1.92055429834348));
#6988=CARTESIAN_POINT('Ctrl Pts',(11.,4.60994183541066,1.96322520805592));
#6989=CARTESIAN_POINT('Ctrl Pts',(11.,4.68054091417581,2.00502145315738));
#6990=CARTESIAN_POINT('Ctrl Pts',(11.,4.75319300565908,2.04321554640376));
#6991=CARTESIAN_POINT('Ctrl Pts',(11.,4.8276935472168,2.07750853757716));
#6992=CARTESIAN_POINT('Ctrl Pts',(11.,4.84971666822096,2.08764589602336));
#6993=CARTESIAN_POINT('Ctrl Pts',(11.,4.87190134628269,2.09744201703478));
#6994=CARTESIAN_POINT('Ctrl Pts',(11.,4.894242333991,2.10688830013711));
#6995=CARTESIAN_POINT('Ctrl Pts',(11.,4.91136213968559,2.11412694747713));
#6996=CARTESIAN_POINT('Ctrl Pts',(11.,4.92857373206428,2.12116015855725));
#6997=CARTESIAN_POINT('Ctrl Pts',(11.,4.94587474276473,2.12798389426578));
#6998=CARTESIAN_POINT('Ctrl Pts',(11.,4.95784258387274,2.13270416096792));
#6999=CARTESIAN_POINT('Ctrl Pts',(11.,4.96985037892949,2.13732300901462));
#7000=CARTESIAN_POINT('Ctrl Pts',(11.,4.98188766633085,2.14183578609736));
#7001=CARTESIAN_POINT('Ctrl Pts',(11.,5.05807742653212,2.1703993147655));
#7002=CARTESIAN_POINT('Ctrl Pts',(11.,5.13555879779739,2.19476158193379));
#7003=CARTESIAN_POINT('Ctrl Pts',(11.,5.21411802734496,2.21467977829964));
#7004=CARTESIAN_POINT('Ctrl Pts',(11.,5.23291149806021,2.21944474407461));
#7005=CARTESIAN_POINT('Ctrl Pts',(11.,5.25176670167758,2.22395514964206));
#7006=CARTESIAN_POINT('Ctrl Pts',(11.,5.27068078412276,2.22820722848632));
#7007=CARTESIAN_POINT('Ctrl Pts',(11.,5.35116102401766,2.24630000810856));
#7008=CARTESIAN_POINT('Ctrl Pts',(11.,5.43270762797145,2.25971979742273));
#7009=CARTESIAN_POINT('Ctrl Pts',(11.,5.51494305755207,2.26856875626421));
#7010=CARTESIAN_POINT('Ctrl Pts',(11.,5.59661107854833,2.27735665899842));
#7011=CARTESIAN_POINT('Ctrl Pts',(11.,5.67895943723679,2.28163617924203));
#7012=CARTESIAN_POINT('Ctrl Pts',(11.,5.76160564919763,2.28145921133302));
#7013=CARTESIAN_POINT('Ctrl Pts',(11.,5.78186348856166,2.28141583381591));
#7014=CARTESIAN_POINT('Ctrl Pts',(11.,5.80213912408603,2.28110449219973));
#7015=CARTESIAN_POINT('Ctrl Pts',(11.,5.82242670183261,2.28052554761898));
#7016=CARTESIAN_POINT('Ctrl Pts',(11.,5.83510702244445,2.28016369057562));
#7017=CARTESIAN_POINT('Ctrl Pts',(11.,5.84779126773273,2.279697238232));
#7018=CARTESIAN_POINT('Ctrl Pts',(11.,5.86046497453528,2.27912708463001));
#7019=CARTESIAN_POINT('Ctrl Pts',(11.,5.94193573517864,2.27546194953095));
#7020=CARTESIAN_POINT('Ctrl Pts',(11.,6.02311364079001,2.26751240450731));
#7021=CARTESIAN_POINT('Ctrl Pts',(11.,6.10364003765459,2.25539767789523));
#7022=CARTESIAN_POINT('Ctrl Pts',(11.,6.1840010683229,2.24330782966262));
#7023=CARTESIAN_POINT('Ctrl Pts',(11.,6.26371425736774,2.22706947431953));
#7024=CARTESIAN_POINT('Ctrl Pts',(11.,6.3424068145887,2.20675222785943));
#7025=CARTESIAN_POINT('Ctrl Pts',(11.,6.41967103165265,2.1868037575584));
#7026=CARTESIAN_POINT('Ctrl Pts',(11.,6.4959521525711,2.1629226440025));
#7027=CARTESIAN_POINT('Ctrl Pts',(11.,6.57086824905388,2.13513440109465));
#7028=CARTESIAN_POINT('Ctrl Pts',(11.,6.60273655364754,2.12331365454369));
#7029=CARTESIAN_POINT('Ctrl Pts',(11.,6.63435741757429,2.11078543462592));
#7030=CARTESIAN_POINT('Ctrl Pts',(11.,6.66569925751203,2.0975497444889));
#7031=CARTESIAN_POINT('Ctrl Pts',(11.,6.67839502656549,2.09218830860714));
#7032=CARTESIAN_POINT('Ctrl Pts',(11.,6.69104621760511,2.08671013926857));
#7033=CARTESIAN_POINT('Ctrl Pts',(11.,6.70363420806782,2.08112276730685));
#7034=CARTESIAN_POINT('Ctrl Pts',(11.,6.77529401289249,2.04931546768698));
#7035=CARTESIAN_POINT('Ctrl Pts',(11.,6.84503127970776,2.0139218522668));
#7036=CARTESIAN_POINT('Ctrl Pts',(11.,6.91250997861022,1.97501181763712));
#7037=CARTESIAN_POINT('Ctrl Pts',(11.,6.97881475247944,1.93677869978917));
#7038=CARTESIAN_POINT('Ctrl Pts',(11.,7.04293957659776,1.89514998025919));
#7039=CARTESIAN_POINT('Ctrl Pts',(11.,7.10453240739252,1.850155007327));
#7040=CARTESIAN_POINT('Ctrl Pts',(11.,7.16414024895716,1.8066101144695));
#7041=CARTESIAN_POINT('Ctrl Pts',(11.,7.22137713707371,1.75991198779978));
#7042=CARTESIAN_POINT('Ctrl Pts',(11.,7.27588415466789,1.71005912218383));
#7043=CARTESIAN_POINT('Ctrl Pts',(11.,7.29498429594792,1.69258987109458));
#7044=CARTESIAN_POINT('Ctrl Pts',(11.,7.31374883354313,1.67473301722448));
#7045=CARTESIAN_POINT('Ctrl Pts',(11.,7.33216095377102,1.65648779355698));
#7046=CARTESIAN_POINT('Ctrl Pts',(11.,7.34331288097895,1.64543695293058));
#7047=CARTESIAN_POINT('Ctrl Pts',(11.,7.3543355061197,1.63424362832598));
#7048=CARTESIAN_POINT('Ctrl Pts',(11.,7.36522742428746,1.62291062336284));
#7049=CARTESIAN_POINT('Origin',(-1.7667098902285,6.,0.));
#7050=CARTESIAN_POINT('Ctrl Pts',(0.233290109771496,8.56244188004781,0.00169655094858908));
#7051=CARTESIAN_POINT('Ctrl Pts',(0.238897060498093,8.56333297831645,0.114092648848322));
#7052=CARTESIAN_POINT('Ctrl Pts',(0.286660438824881,8.50572313696992,1.07067066579831));
#7053=CARTESIAN_POINT('Ctrl Pts',(0.376580244751861,7.30166397004841,2.72694193252232));
#7054=CARTESIAN_POINT('Ctrl Pts',(0.503049527552434,4.42618944743245,2.57901724514726));
#7055=CARTESIAN_POINT('Ctrl Pts',(0.629518810353006,2.97989373731284,0.0895594277083228));
#7056=CARTESIAN_POINT('Ctrl Pts',(0.755988093153581,4.27624391707079,-2.48150710395807));
#7057=CARTESIAN_POINT('Ctrl Pts',(0.882457375954154,7.13796708616038,-2.79891497944178));
#7058=CARTESIAN_POINT('Ctrl Pts',(0.974891381493459,8.47424725723099,-1.17323432323149));
#7059=CARTESIAN_POINT('Ctrl Pts',(1.02516895943257,8.56249188360061,-0.165257813814287));
#7060=CARTESIAN_POINT('Ctrl Pts',(1.0332901097715,8.5610206941956,-0.00218674593362883));
#7061=CARTESIAN_POINT('Ctrl Pts',(0.166709890228505,8.55738198002468,-0.00304066224802793));
#7062=CARTESIAN_POINT('Ctrl Pts',(0.195452782019385,8.55313914952871,0.576034719477703));
#7063=CARTESIAN_POINT('Ctrl Pts',(0.266352101410457,8.07386839878632,2.0128937423642));
#7064=CARTESIAN_POINT('Ctrl Pts',(0.379407848401719,5.69862372086684,3.00550592532682));
#7065=CARTESIAN_POINT('Ctrl Pts',(0.505877131202292,3.31720488565003,1.38974961778526));
#7066=CARTESIAN_POINT('Ctrl Pts',(0.632346414002866,3.37108102552373,-1.4897402431435));
#7067=CARTESIAN_POINT('Ctrl Pts',(0.758815696803437,5.81286715979806,-3.01549246530217));
#7068=CARTESIAN_POINT('Ctrl Pts',(0.870270188878652,8.11427830150227,-1.94718071880993));
#7069=CARTESIAN_POINT('Ctrl Pts',(0.939568253353674,8.5537603444746,-0.545331335115959));
#7070=CARTESIAN_POINT('Ctrl Pts',(0.966709890228505,8.55722909061475,0.00173622970309435));
#7071=CARTESIAN_POINT('Ctrl Pts',(-2.77555756156289E-16,4.38007430561128,
1.36291222925734));
#7072=CARTESIAN_POINT('Ctrl Pts',(0.0421564276001907,3.92881977966068,0.826561622369841));
#7073=CARTESIAN_POINT('Ctrl Pts',(0.126469282800573,3.60822370236051,-0.720174349784107));
#7074=CARTESIAN_POINT('Ctrl Pts',(0.252938565601145,5.30081920607079,-2.40042716259123));
#7075=CARTESIAN_POINT('Ctrl Pts',(0.37940784840172,7.62787861345926,-1.89456883750813));
#7076=CARTESIAN_POINT('Ctrl Pts',(0.505877131202291,8.47683544733721,0.328672733398138));
#7077=CARTESIAN_POINT('Ctrl Pts',(0.632346414002866,7.07641508773143,2.25505315279287));
#7078=CARTESIAN_POINT('Ctrl Pts',(0.758815696803438,4.69853244539629,2.13272637030342));
#7079=CARTESIAN_POINT('Ctrl Pts',(0.885284979604012,3.50251368823877,0.0740614486166079));
#7080=CARTESIAN_POINT('Ctrl Pts',(1.01175426240458,4.57453452048393,-2.05209005432782));
#7081=CARTESIAN_POINT('Ctrl Pts',(1.13822354520516,6.94104543804747,-2.31457148885869));
#7082=CARTESIAN_POINT('Ctrl Pts',(1.26469282800573,8.45297548944686,-0.4752001569218));
#7083=CARTESIAN_POINT('Ctrl Pts',(1.3911621108063,7.73730008478527,1.79574410473392));
#7084=CARTESIAN_POINT('Ctrl Pts',(1.51763139360688,5.44394372984514,2.43591482501934));
#7085=CARTESIAN_POINT('Ctrl Pts',(1.64410067640745,3.65555424849459,0.863984350743103));
#7086=CARTESIAN_POINT('Ctrl Pts',(1.77056995920802,3.99621004749271,-1.49255480899735));
#7087=CARTESIAN_POINT('Ctrl Pts',(1.8970392420086,6.1565533162993,-2.49366826061349));
#7088=CARTESIAN_POINT('Ctrl Pts',(2.02350852480917,8.17472700992591,-1.23022562847364));
#7089=CARTESIAN_POINT('Ctrl Pts',(2.14997780760974,8.21798116746057,1.15041378883214));
#7090=CARTESIAN_POINT('Ctrl Pts',(2.27644709041031,6.24703576222385,2.48633570206331));
#7091=CARTESIAN_POINT('Ctrl Pts',(2.40291637321089,4.05175150168771,1.56435930211391));
#7092=CARTESIAN_POINT('Ctrl Pts',(2.52938565601146,3.62571640747785,-0.778247766418806));
#7093=CARTESIAN_POINT('Ctrl Pts',(2.65585493881203,5.35582271376271,-2.41411013316777));
#7094=CARTESIAN_POINT('Ctrl Pts',(2.78232422161261,7.67092119477938,-1.8576637268496));
#7095=CARTESIAN_POINT('Ctrl Pts',(2.90879350441318,8.46861780186369,0.385769743907112));
#7096=CARTESIAN_POINT('Ctrl Pts',(3.03526278721376,7.02450594585644,2.27887685238754));
#7097=CARTESIAN_POINT('Ctrl Pts',(3.16173207001433,4.65001673485963,2.1024836104791));
#7098=CARTESIAN_POINT('Ctrl Pts',(3.2882013528149,3.5014782998291,0.0167767625214216));
#7099=CARTESIAN_POINT('Ctrl Pts',(3.41467063561547,4.62190474442643,-2.08416544738097));
#7100=CARTESIAN_POINT('Ctrl Pts',(3.54113991841605,6.9938111083862,-2.29242919788285));
#7101=CARTESIAN_POINT('Ctrl Pts',(3.66760920121662,8.46321480372051,-0.418885398138105));
#7102=CARTESIAN_POINT('Ctrl Pts',(3.7940784840172,7.69571662208578,1.8350578420303));
#7103=CARTESIAN_POINT('Ctrl Pts',(3.92054776681776,5.38829927097786,2.42254295405827));
#7104=CARTESIAN_POINT('Ctrl Pts',(4.04701704961834,3.63638138619269,0.810061228883945));
#7105=CARTESIAN_POINT('Ctrl Pts',(4.17348633241891,4.03091979328168,-1.53805568351414));
#7106=CARTESIAN_POINT('Ctrl Pts',(4.29995561521948,6.21362511284545,-2.48942894199821));
#7107=CARTESIAN_POINT('Ctrl Pts',(4.42642489802006,8.20233256621709,-1.18009466309531));
#7108=CARTESIAN_POINT('Ctrl Pts',(4.55289418082062,8.19105128792784,1.20091065436085));
#7109=CARTESIAN_POINT('Ctrl Pts',(4.67936346362121,6.1900260656191,2.49134145401128));
#7110=CARTESIAN_POINT('Ctrl Pts',(4.80583274642177,4.01643381333958,1.51932792024159));
#7111=CARTESIAN_POINT('Ctrl Pts',(4.93230202922236,3.64416352427244,-0.832422155952186));
#7112=CARTESIAN_POINT('Ctrl Pts',(5.05877131202292,5.41128238894444,-2.42823057400276));
#7113=CARTESIAN_POINT('Ctrl Pts',(5.1852405948235,7.71302922320777,-1.81890709672723));
#7114=CARTESIAN_POINT('Ctrl Pts',(5.31170987762407,8.45913491771966,0.442207646406598));
#7115=CARTESIAN_POINT('Ctrl Pts',(5.43817916042464,6.97204377333561,2.30174348023582));
#7116=CARTESIAN_POINT('Ctrl Pts',(5.56464844322521,4.60221737671311,2.07101325059156));
#7117=CARTESIAN_POINT('Ctrl Pts',(5.6911177260258,3.50174944972781,-0.0404516273254309));
#7118=CARTESIAN_POINT('Ctrl Pts',(5.81758700882635,4.67000016499225,-2.11518145438353));
#7119=CARTESIAN_POINT('Ctrl Pts',(5.94405629162694,7.04605424471208,-2.26906647395101));
#7120=CARTESIAN_POINT('Ctrl Pts',(6.07052557442751,8.47216246510873,-0.362360169163266));
#7121=CARTESIAN_POINT('Ctrl Pts',(6.19699485722808,7.65324323193351,1.87341371889789));
#7122=CARTESIAN_POINT('Ctrl Pts',(6.32346414002865,5.33297588935731,2.40789762695798));
#7123=CARTESIAN_POINT('Ctrl Pts',(6.44993342282923,3.61844844523957,0.755714455403861));
#7124=CARTESIAN_POINT('Ctrl Pts',(6.5764027056298,4.0666626081133,-1.5827503515155));
#7125=CARTESIAN_POINT('Ctrl Pts',(6.70287198843037,6.27058481326315,-2.48388325106456));
#7126=CARTESIAN_POINT('Ctrl Pts',(6.82934127123095,8.22878274143999,-1.1293447824051));
#7127=CARTESIAN_POINT('Ctrl Pts',(6.95581055403152,8.16297192699002,1.25077759379901));
#7128=CARTESIAN_POINT('Ctrl Pts',(7.08227983683209,6.13291668041033,2.49504014038827));
#7129=CARTESIAN_POINT('Ctrl Pts',(7.20874911963267,3.98215674684198,1.47349949160562));
#7130=CARTESIAN_POINT('Ctrl Pts',(7.33521840243324,3.66384656697614,-0.886159852122868));
#7131=CARTESIAN_POINT('Ctrl Pts',(7.46168768523381,5.46705091821445,-2.44107710288693));
#7132=CARTESIAN_POINT('Ctrl Pts',(7.58815696803438,7.75423855804789,-1.77919623074557));
#7133=CARTESIAN_POINT('Ctrl Pts',(7.71462625083496,8.44836191581642,0.498413558841803));
#7134=CARTESIAN_POINT('Ctrl Pts',(7.84109553363553,6.91907164464643,2.32340256036229));
#7135=CARTESIAN_POINT('Ctrl Pts',(7.9675648164361,4.55515132709709,2.03845639109507));
#7136=CARTESIAN_POINT('Ctrl Pts',(8.09403409923669,3.50333123781422,-0.0976587959070175));
#7137=CARTESIAN_POINT('Ctrl Pts',(8.22050338203724,4.71879333438784,-2.14508778874756));
#7138=CARTESIAN_POINT('Ctrl Pts',(8.34697266483783,7.0977485956482,-2.2445133476424));
#7139=CARTESIAN_POINT('Ctrl Pts',(8.47344194763839,8.47981317754976,-0.305644835824586));
#7140=CARTESIAN_POINT('Ctrl Pts',(8.59991123043898,7.60990250675094,1.91078675679009));
#7141=CARTESIAN_POINT('Ctrl Pts',(8.72638051323954,5.27800245571656,2.3919890697293));
#7142=CARTESIAN_POINT('Ctrl Pts',(8.85284979604011,3.60176489689208,0.700971203051395));
#7143=CARTESIAN_POINT('Ctrl Pts',(8.9793190788407,4.10341973960911,-1.62661464614942));
#7144=CARTESIAN_POINT('Ctrl Pts',(9.10578836164126,6.32740247414682,-2.47703451018903));
#7145=CARTESIAN_POINT('Ctrl Pts',(9.23225764444184,8.25406380889129,-1.07800232379207));
#7146=CARTESIAN_POINT('Ctrl Pts',(9.35872692724241,8.13375751216227,1.29998815922553));
#7147=CARTESIAN_POINT('Ctrl Pts',(9.48519621004298,6.0757381573693,2.4974302318881));
#7148=CARTESIAN_POINT('Ctrl Pts',(9.61166549284355,3.94893715107484,1.4268973438337));
#7149=CARTESIAN_POINT('Ctrl Pts',(9.73813477564413,3.68475738146131,-0.93943133204598));
#7150=CARTESIAN_POINT('Ctrl Pts',(9.86460405844469,5.52309488595575,-2.45264550770796));
#7151=CARTESIAN_POINT('Ctrl Pts',(9.99107334124528,7.79453553867095,-1.73854713522886));
#7152=CARTESIAN_POINT('Ctrl Pts',(10.1175426240458,8.43628921595103,0.554348761835227));
#7153=CARTESIAN_POINT('Ctrl Pts',(10.2440119068464,6.86564650173235,2.34386039652572));
#7154=CARTESIAN_POINT('Ctrl Pts',(10.370481189647,4.50878748634398,2.00479630255084));
#7155=CARTESIAN_POINT('Ctrl Pts',(10.4969504724476,3.50632961359115,-0.154750024947643));
#7156=CARTESIAN_POINT('Ctrl Pts',(10.6234197552481,4.76805426261496,-2.1739926088089));
#7157=CARTESIAN_POINT('Ctrl Pts',(10.7498890380487,7.1492585246536,-2.21854556914584));
#7158=CARTESIAN_POINT('Ctrl Pts',(10.8763583208493,8.48541088840014,-0.249223947559238));
#7159=CARTESIAN_POINT('Ctrl Pts',(11.0028276036499,7.56718166314935,1.94803644221398));
#7160=CARTESIAN_POINT('Ctrl Pts',(11.1292968864504,5.22037961200964,2.37306489642968));
#7161=CARTESIAN_POINT('Ctrl Pts',(11.2136097416508,4.13613327342382,1.22433347020397));
#7162=CARTESIAN_POINT('Ctrl Pts',(11.255766169251,3.95494913733603,0.547225702171725));
#7163=CARTESIAN_POINT('Ctrl Pts',(-0.085255389750335,4.26707996100189,1.45797916636347));
#7164=CARTESIAN_POINT('Ctrl Pts',(-0.043098962150144,3.78434917068409,0.884216605633869));
#7165=CARTESIAN_POINT('Ctrl Pts',(0.0412138930502387,3.44139062097895,-0.770408523450359));
#7166=CARTESIAN_POINT('Ctrl Pts',(0.167683175850811,5.25204939159895,-2.56786366598092));
#7167=CARTESIAN_POINT('Ctrl Pts',(0.294152458651385,7.74142769640091,-2.0267203089325));
#7168=CARTESIAN_POINT('Ctrl Pts',(0.420621741451956,8.64960164213652,0.35159857513887));
#7169=CARTESIAN_POINT('Ctrl Pts',(0.547091024252532,7.15149804850376,2.41234941270269));
#7170=CARTESIAN_POINT('Ctrl Pts',(0.673560307053103,4.60775144607501,2.28148999525137));
#7171=CARTESIAN_POINT('Ctrl Pts',(0.800029589853676,3.32830703793013,0.0792274416471788));
#7172=CARTESIAN_POINT('Ctrl Pts',(0.92649887265425,4.47510431934622,-2.19522907087124));
#7173=CARTESIAN_POINT('Ctrl Pts',(1.05296815545482,7.00668598741845,-2.47601931905305));
#7174=CARTESIAN_POINT('Ctrl Pts',(1.1794374382554,8.62407738549864,-0.508346695973345));
#7175=CARTESIAN_POINT('Ctrl Pts',(1.30590672105597,7.85848162116695,1.92100227484841));
#7176=CARTESIAN_POINT('Ctrl Pts',(1.43237600385654,5.40515725091604,2.60582669204557));
#7177=CARTESIAN_POINT('Ctrl Pts',(1.55884528665711,3.49202260498698,0.924249673901536));
#7178=CARTESIAN_POINT('Ctrl Pts',(1.68531456945769,3.8564400980421,-1.59666467837002));
#7179=CARTESIAN_POINT('Ctrl Pts',(1.81178385225826,6.16747334765195,-2.66760859118376));
#7180=CARTESIAN_POINT('Ctrl Pts',(1.93825313505883,8.32642029687239,-1.31603730433789));
#7181=CARTESIAN_POINT('Ctrl Pts',(2.06472241785941,8.37269155278336,1.23065836582043));
#7182=CARTESIAN_POINT('Ctrl Pts',(2.19119170065998,6.26426719706327,2.65976456618141));
#7183=CARTESIAN_POINT('Ctrl Pts',(2.31766098346055,3.91585572389644,1.6734777355632));
#7184=CARTESIAN_POINT('Ctrl Pts',(2.44413026626112,3.46010349116746,-0.832532723200972));
#7185=CARTESIAN_POINT('Ctrl Pts',(2.5705995490617,5.31088954767814,-2.58250106199683));
#7186=CARTESIAN_POINT('Ctrl Pts',(2.69706883186227,7.78747261806504,-1.98724096366182));
#7187=CARTESIAN_POINT('Ctrl Pts',(2.82353811466285,8.64081079292425,0.412678261707595));
#7188=CARTESIAN_POINT('Ctrl Pts',(2.95000739746342,7.09596809890546,2.4378348819274));
#7189=CARTESIAN_POINT('Ctrl Pts',(3.07647668026399,4.555851629135,2.24913771840577));
#7190=CARTESIAN_POINT('Ctrl Pts',(3.20294596306457,3.32719942828513,0.0179469885955816));
#7191=CARTESIAN_POINT('Ctrl Pts',(3.32941524586514,4.52577874880069,-2.22954181223529));
#7192=CARTESIAN_POINT('Ctrl Pts',(3.45588452866571,7.06313221073467,-2.45233254139759));
#7193=CARTESIAN_POINT('Ctrl Pts',(3.58235381146628,8.63503092056008,-0.448103825374002));
#7194=CARTESIAN_POINT('Ctrl Pts',(3.70882309426686,7.81399759572522,1.96305825519663));
#7195=CARTESIAN_POINT('Ctrl Pts',(3.83529237706742,5.34563143552567,2.59152209571278));
#7196=CARTESIAN_POINT('Ctrl Pts',(3.96176165986801,3.47151238195452,0.866565263586447));
#7197=CARTESIAN_POINT('Ctrl Pts',(4.08823094266858,3.89357094560789,-1.64533936605182));
#7198=CARTESIAN_POINT('Ctrl Pts',(4.21470022546915,6.22852606151346,-2.66307356824687));
#7199=CARTESIAN_POINT('Ctrl Pts',(4.34116950826973,8.35595141786789,-1.26240956401662));
#7200=CARTESIAN_POINT('Ctrl Pts',(4.4676387910703,8.34388323888864,1.28467752885019));
#7201=CARTESIAN_POINT('Ctrl Pts',(4.59410807387086,6.20328091478762,2.66511948331801));
#7202=CARTESIAN_POINT('Ctrl Pts',(4.72057735667144,3.87807452807889,1.62530528894999));
#7203=CARTESIAN_POINT('Ctrl Pts',(4.84704663947202,3.47983734591513,-0.890485927812807));
#7204=CARTESIAN_POINT('Ctrl Pts',(4.97351592227259,5.37021769020446,-2.59760644304437));
#7205=CARTESIAN_POINT('Ctrl Pts',(5.09998520507316,7.83251779916133,-1.94578095027001));
#7206=CARTESIAN_POINT('Ctrl Pts',(5.22645448787373,8.63066645110808,0.473052865641068));
#7207=CARTESIAN_POINT('Ctrl Pts',(5.35292377067431,7.03984654322817,2.46229652097656));
#7208=CARTESIAN_POINT('Ctrl Pts',(5.47939305347488,4.50471813216642,2.21547221296159));
#7209=CARTESIAN_POINT('Ctrl Pts',(5.60586233627545,3.32748949164709,-0.0432732413870235));
#7210=CARTESIAN_POINT('Ctrl Pts',(5.73233161907602,4.57722895936978,-2.26272127241091));
#7211=CARTESIAN_POINT('Ctrl Pts',(5.8588009018766,7.11901945183022,-2.42734020217653));
#7212=CARTESIAN_POINT('Ctrl Pts',(5.98527018467717,8.64460270633739,-0.387635803699455));
#7213=CARTESIAN_POINT('Ctrl Pts',(6.11173946747775,7.76856156790366,2.00408956167411));
#7214=CARTESIAN_POINT('Ctrl Pts',(6.23820875027831,5.28644909341736,2.57585521611596));
#7215=CARTESIAN_POINT('Ctrl Pts',(6.3646780330789,3.45232856825029,0.808427650765839));
#7216=CARTESIAN_POINT('Ctrl Pts',(6.49114731587947,3.9318069216693,-1.69315161206052));
#7217=CARTESIAN_POINT('Ctrl Pts',(6.61761659868004,6.2894588602283,-2.65714104987129));
#7218=CARTESIAN_POINT('Ctrl Pts',(6.74408588148061,8.38424656673646,-1.2081197373107));
#7219=CARTESIAN_POINT('Ctrl Pts',(6.87055516428118,8.31384526404822,1.33802282668406));
#7220=CARTESIAN_POINT('Ctrl Pts',(6.99702444708176,6.14218799034921,2.66907616340701));
#7221=CARTESIAN_POINT('Ctrl Pts',(7.12349372988232,3.84140654039433,1.57628019933373));
#7222=CARTESIAN_POINT('Ctrl Pts',(7.24996301268291,3.50089333585828,-0.947971978479414));
#7223=CARTESIAN_POINT('Ctrl Pts',(7.37643229548348,5.42987623025491,-2.61134905322214));
#7224=CARTESIAN_POINT('Ctrl Pts',(7.50290157828404,7.87660160027986,-1.90330014040079));
#7225=CARTESIAN_POINT('Ctrl Pts',(7.62937086108463,8.61914200221331,0.533179297554908));
#7226=CARTESIAN_POINT('Ctrl Pts',(7.75584014388519,6.98317946051453,2.48546638247541));
#7227=CARTESIAN_POINT('Ctrl Pts',(7.88230942668577,4.45436909404781,2.18064442152415));
#7228=CARTESIAN_POINT('Ctrl Pts',(8.00877870948634,3.32918161387337,-0.104470769861797));
#7229=CARTESIAN_POINT('Ctrl Pts',(8.13524799228692,4.62942558869958,-2.29471365718012));
#7230=CARTESIAN_POINT('Ctrl Pts',(8.26171727508748,7.17431962822135,-2.40107442668595));
#7231=CARTESIAN_POINT('Ctrl Pts',(8.38818655788806,8.65278707735367,-0.326964417350377));
#7232=CARTESIAN_POINT('Ctrl Pts',(8.51465584068864,7.72219770600942,2.04406947341078));
#7233=CARTESIAN_POINT('Ctrl Pts',(8.64112512348921,5.22764110913847,2.55883699255878));
#7234=CARTESIAN_POINT('Ctrl Pts',(8.76759440628978,3.43448129577779,0.749865903563404));
#7235=CARTESIAN_POINT('Ctrl Pts',(8.89406368909035,3.97112796581709,-1.74007556383864));
#7236=CARTESIAN_POINT('Ctrl Pts',(9.02053297189094,6.35023971175459,-2.6498145901786));
#7237=CARTESIAN_POINT('Ctrl Pts',(9.14700225469149,8.41129105929893,-1.15319599871568));
#7238=CARTESIAN_POINT('Ctrl Pts',(9.27347153749208,8.28259306213672,1.39066596658451));
#7239=CARTESIAN_POINT('Ctrl Pts',(9.39994082029264,6.08102110552151,2.67163297046886));
#7240=CARTESIAN_POINT('Ctrl Pts',(9.52641010309322,3.80586978497912,1.5264274215094));
#7241=CARTESIAN_POINT('Ctrl Pts',(9.65287938589379,3.52326273809608,-1.00495929301219));
#7242=CARTESIAN_POINT('Ctrl Pts',(9.77934866869437,5.48982942137984,-2.62372438661122));
#7243=CARTESIAN_POINT('Ctrl Pts',(9.90581795149493,7.91970940792481,-1.85981565686425));
#7244=CARTESIAN_POINT('Ctrl Pts',(10.0322872342955,8.60622719779109,0.593016137286807));
#7245=CARTESIAN_POINT('Ctrl Pts',(10.1587565170961,6.92602776456773,2.50735120988754));
#7246=CARTESIAN_POINT('Ctrl Pts',(10.2852257998967,4.40477124582285,2.14463644772956));
#7247=CARTESIAN_POINT('Ctrl Pts',(10.4116950826972,3.33238913474072,-0.165544271688598));
#7248=CARTESIAN_POINT('Ctrl Pts',(10.5381643654978,4.68212260434671,-2.32563466922495));
#7249=CARTESIAN_POINT('Ctrl Pts',(10.6646336482984,7.22942251873667,-2.37329532306358));
#7250=CARTESIAN_POINT('Ctrl Pts',(10.7911029310989,8.65877524418052,-0.266608014441423));
#7251=CARTESIAN_POINT('Ctrl Pts',(10.9175722138995,7.6764969641689,2.08391742849973));
#7252=CARTESIAN_POINT('Ctrl Pts',(11.0440414967001,5.1659989110366,2.53859280528157));
#7253=CARTESIAN_POINT('Ctrl Pts',(11.1283543519005,4.00612336004432,1.30973415156129));
#7254=CARTESIAN_POINT('Ctrl Pts',(11.1705107795007,3.81230112408455,0.585396224303999));
#7255=CARTESIAN_POINT('Ctrl Pts',(-0.17051077950067,4.15408561639251,1.55304610346959));
#7256=CARTESIAN_POINT('Ctrl Pts',(-0.128354351900479,3.6398785617075,0.941871588897895));
#7257=CARTESIAN_POINT('Ctrl Pts',(-0.0440414967000963,3.27455753959738,
-0.820642697116609));
#7258=CARTESIAN_POINT('Ctrl Pts',(0.0824277861004764,5.20327957712712,-2.73530016937061));
#7259=CARTESIAN_POINT('Ctrl Pts',(0.20889706890105,7.85497677934257,-2.15887178035685));
#7260=CARTESIAN_POINT('Ctrl Pts',(0.335366351701623,8.82236783693583,0.374524416879597));
#7261=CARTESIAN_POINT('Ctrl Pts',(0.461835634502195,7.22658100927608,2.56964567261251));
#7262=CARTESIAN_POINT('Ctrl Pts',(0.588304917302769,4.51697044675373,2.43025362019932));
#7263=CARTESIAN_POINT('Ctrl Pts',(0.714774200103341,3.15410038762148,0.0843934346777503));
#7264=CARTESIAN_POINT('Ctrl Pts',(0.841243482903915,4.3756741182085,-2.33836808741465));
#7265=CARTESIAN_POINT('Ctrl Pts',(0.967712765704489,7.07232653678942,-2.63746714924742));
#7266=CARTESIAN_POINT('Ctrl Pts',(1.09418204850506,8.79517928155045,-0.541493235024889));
#7267=CARTESIAN_POINT('Ctrl Pts',(1.22065133130563,7.97966315754858,2.0462604449629));
#7268=CARTESIAN_POINT('Ctrl Pts',(1.34712061410621,5.36637077198697,2.77573855907179));
#7269=CARTESIAN_POINT('Ctrl Pts',(1.47358989690678,3.32849096147935,0.984514997059966));
#7270=CARTESIAN_POINT('Ctrl Pts',(1.60005917970736,3.71667014859151,-1.70077454774269));
#7271=CARTESIAN_POINT('Ctrl Pts',(1.72652846250793,6.17839337900458,-2.84154892175403));
#7272=CARTESIAN_POINT('Ctrl Pts',(1.8529977453085,8.47811358381889,-1.40184898020213));
#7273=CARTESIAN_POINT('Ctrl Pts',(1.97946702810908,8.52740193810615,1.31090294280873));
#7274=CARTESIAN_POINT('Ctrl Pts',(2.10593631090964,6.28149863190269,2.83319343029951));
#7275=CARTESIAN_POINT('Ctrl Pts',(2.23240559371022,3.77995994610518,1.7825961690125));
#7276=CARTESIAN_POINT('Ctrl Pts',(2.35887487651079,3.29449057485706,-0.886817679983138));
#7277=CARTESIAN_POINT('Ctrl Pts',(2.48534415931137,5.26595638159357,-2.75089199082588));
#7278=CARTESIAN_POINT('Ctrl Pts',(2.61181344211193,7.9040240413507,-2.11681820047403));
#7279=CARTESIAN_POINT('Ctrl Pts',(2.73828272491252,8.81300378398482,0.439586779508076));
#7280=CARTESIAN_POINT('Ctrl Pts',(2.86475200771308,7.1674302519545,2.59679291146726));
#7281=CARTESIAN_POINT('Ctrl Pts',(2.99122129051366,4.46168652341036,2.39579182633243));
#7282=CARTESIAN_POINT('Ctrl Pts',(3.11769057331423,3.15292055674116,0.0191172146697414));
#7283=CARTESIAN_POINT('Ctrl Pts',(3.2441598561148,4.42965275317496,-2.37491817708961));
#7284=CARTESIAN_POINT('Ctrl Pts',(3.37062913891538,7.13245331308311,-2.61223588491233));
#7285=CARTESIAN_POINT('Ctrl Pts',(3.49709842171594,8.80684703739969,-0.477322252609899));
#7286=CARTESIAN_POINT('Ctrl Pts',(3.62356770451653,7.93227856936462,2.09105866836297));
#7287=CARTESIAN_POINT('Ctrl Pts',(3.7500369873171,5.30296360007351,2.7605012373673));
#7288=CARTESIAN_POINT('Ctrl Pts',(3.87650627011767,3.30664337771634,0.923069298288947));
#7289=CARTESIAN_POINT('Ctrl Pts',(4.00297555291824,3.75622209793411,-1.75262304858949));
#7290=CARTESIAN_POINT('Ctrl Pts',(4.12944483571881,6.24342701018146,-2.83671819449552));
#7291=CARTESIAN_POINT('Ctrl Pts',(4.2559141185194,8.50957026951867,-1.34472446493793));
#7292=CARTESIAN_POINT('Ctrl Pts',(4.38238340131996,8.49671518984944,1.36844440333954));
#7293=CARTESIAN_POINT('Ctrl Pts',(4.50885268412054,6.21653576395613,2.83889751262473));
#7294=CARTESIAN_POINT('Ctrl Pts',(4.6353219669211,3.73971524281822,1.73128265765839));
#7295=CARTESIAN_POINT('Ctrl Pts',(4.76179124972169,3.31551116755782,-0.948549699673432));
#7296=CARTESIAN_POINT('Ctrl Pts',(4.88826053252225,5.32915299146447,-2.76698231208597));
#7297=CARTESIAN_POINT('Ctrl Pts',(5.01472981532283,7.9520063751149,-2.07265480381278));
#7298=CARTESIAN_POINT('Ctrl Pts',(5.1411990981234,8.80219798449649,0.503898084875541));
#7299=CARTESIAN_POINT('Ctrl Pts',(5.26766838092398,7.10764931312074,2.62284956171731));
#7300=CARTESIAN_POINT('Ctrl Pts',(5.39413766372455,4.40721888761971,2.35993117533163));
#7301=CARTESIAN_POINT('Ctrl Pts',(5.52060694652512,3.15322953356639,-0.0460948554486148));
#7302=CARTESIAN_POINT('Ctrl Pts',(5.6470762293257,4.48445775374728,-2.41026109043829));
#7303=CARTESIAN_POINT('Ctrl Pts',(5.77354551212626,7.1919846589484,-2.58561393040205));
#7304=CARTESIAN_POINT('Ctrl Pts',(5.90001479492684,8.81704294756603,-0.412911438235641));
#7305=CARTESIAN_POINT('Ctrl Pts',(6.02648407772741,7.88387990387384,2.13476540445033));
#7306=CARTESIAN_POINT('Ctrl Pts',(6.15295336052798,5.23992229747739,2.74381280527395));
#7307=CARTESIAN_POINT('Ctrl Pts',(6.27942264332857,3.28620869126101,0.861140846127814));
#7308=CARTESIAN_POINT('Ctrl Pts',(6.40589192612913,3.79695123522531,-1.80355287260552));
#7309=CARTESIAN_POINT('Ctrl Pts',(6.5323612089297,6.30833290719342,-2.83039884867804));
#7310=CARTESIAN_POINT('Ctrl Pts',(6.65883049173028,8.53971039203294,-1.2868946922163));
#7311=CARTESIAN_POINT('Ctrl Pts',(6.78529977453085,8.4647186011064,1.42526805956911));
#7312=CARTESIAN_POINT('Ctrl Pts',(6.91176905733142,6.15145930028808,2.84311218642574));
#7313=CARTESIAN_POINT('Ctrl Pts',(7.038238340132,3.70065633394668,1.67906090706185));
#7314=CARTESIAN_POINT('Ctrl Pts',(7.16470762293257,3.33794010474041,-1.00978410483596));
#7315=CARTESIAN_POINT('Ctrl Pts',(7.29117690573314,5.39270154229538,-2.78162100355734));
#7316=CARTESIAN_POINT('Ctrl Pts',(7.41764618853372,7.99896464251182,-2.02740405005601));
#7317=CARTESIAN_POINT('Ctrl Pts',(7.54411547133428,8.78992208861021,0.567945036268011));
#7318=CARTESIAN_POINT('Ctrl Pts',(7.67058475413486,7.04728727638264,2.64753020458854));
#7319=CARTESIAN_POINT('Ctrl Pts',(7.79705403693543,4.35358686099853,2.32283245195324));
#7320=CARTESIAN_POINT('Ctrl Pts',(7.92352331973601,3.15503198993253,-0.111282743816577));
#7321=CARTESIAN_POINT('Ctrl Pts',(8.04999260253657,4.54005784301132,-2.44433952561267));
#7322=CARTESIAN_POINT('Ctrl Pts',(8.17646188533716,7.25089066079452,-2.5576355057295));
#7323=CARTESIAN_POINT('Ctrl Pts',(8.30293116813772,8.82576097715756,-0.348283998876166));
#7324=CARTESIAN_POINT('Ctrl Pts',(8.42940045093831,7.83449290526792,2.17735219003147));
#7325=CARTESIAN_POINT('Ctrl Pts',(8.55586973373887,5.17727976256035,2.72568491538827));
#7326=CARTESIAN_POINT('Ctrl Pts',(8.68233901653945,3.26719769466351,0.79876060407541));
#7327=CARTESIAN_POINT('Ctrl Pts',(8.80880829934001,3.83883619202506,-1.85353648152785));
#7328=CARTESIAN_POINT('Ctrl Pts',(8.93527758214061,6.37307694936239,-2.82259467016817));
#7329=CARTESIAN_POINT('Ctrl Pts',(9.06174686494116,8.56851830970655,-1.2283896736393));
#7330=CARTESIAN_POINT('Ctrl Pts',(9.18821614774174,8.4314286121112,1.48134377394349));
#7331=CARTESIAN_POINT('Ctrl Pts',(9.31468543054231,6.0863040536737,2.84583570904962));
#7332=CARTESIAN_POINT('Ctrl Pts',(9.44115471334289,3.66280241888341,1.62595749918509));
#7333=CARTESIAN_POINT('Ctrl Pts',(9.56762399614345,3.36176809473084,-1.07048725397839));
#7334=CARTESIAN_POINT('Ctrl Pts',(9.69409327894404,5.45656395680392,-2.79480326551449));
#7335=CARTESIAN_POINT('Ctrl Pts',(9.8205625617446,8.04488327717867,-1.98108417849965));
#7336=CARTESIAN_POINT('Ctrl Pts',(9.94703184454518,8.77616517963117,0.631683512738392));
#7337=CARTESIAN_POINT('Ctrl Pts',(10.0735011273457,6.98640902740309,2.67084202324935));
#7338=CARTESIAN_POINT('Ctrl Pts',(10.1999704101463,4.30075500530173,2.28447659290827));
#7339=CARTESIAN_POINT('Ctrl Pts',(10.3264396929469,3.15844865589028,-0.176338518429553));
#7340=CARTESIAN_POINT('Ctrl Pts',(10.4529089757475,4.59619094607847,-2.47727672964101));
#7341=CARTESIAN_POINT('Ctrl Pts',(10.579378258548,7.30958651281973,-2.52804507698133));
#7342=CARTESIAN_POINT('Ctrl Pts',(10.7058475413486,8.83213959996092,-0.283992081323606));
#7343=CARTESIAN_POINT('Ctrl Pts',(10.8323168241492,7.78581226518845,2.21979841478548));
#7344=CARTESIAN_POINT('Ctrl Pts',(10.9587861069498,5.11161821006357,2.70412071413346));
#7345=CARTESIAN_POINT('Ctrl Pts',(11.0430989621501,3.87611344666481,1.39513483291862));
#7346=CARTESIAN_POINT('Ctrl Pts',(11.0852553897503,3.66965311083307,0.623566746436274));
#7347=CARTESIAN_POINT('Ctrl Pts',(-0.255766169251004,4.04109127178312,1.64811304057572));
#7348=CARTESIAN_POINT('Ctrl Pts',(-0.213609741650813,3.49540795273091,0.999526572161923));
#7349=CARTESIAN_POINT('Ctrl Pts',(-0.129296886450431,3.10772445821582,-0.870876870782859));
#7350=CARTESIAN_POINT('Ctrl Pts',(-0.00282760364985834,5.15450976265528,
-2.9027366727603));
#7351=CARTESIAN_POINT('Ctrl Pts',(0.123641679150715,7.96852586228423,-2.29102325178121));
#7352=CARTESIAN_POINT('Ctrl Pts',(0.250110961951288,8.99513403173513,0.397450258620327));
#7353=CARTESIAN_POINT('Ctrl Pts',(0.376580244751861,7.30166397004841,2.72694193252232));
#7354=CARTESIAN_POINT('Ctrl Pts',(0.503049527552434,4.42618944743245,2.57901724514726));
#7355=CARTESIAN_POINT('Ctrl Pts',(0.629518810353006,2.97989373731284,0.0895594277083228));
#7356=CARTESIAN_POINT('Ctrl Pts',(0.755988093153581,4.27624391707079,-2.48150710395807));
#7357=CARTESIAN_POINT('Ctrl Pts',(0.882457375954154,7.13796708616038,-2.79891497944178));
#7358=CARTESIAN_POINT('Ctrl Pts',(1.00892665875473,8.96628117760225,-0.574639774076433));
#7359=CARTESIAN_POINT('Ctrl Pts',(1.1353959415553,8.10084469393023,2.17151861507739));
#7360=CARTESIAN_POINT('Ctrl Pts',(1.26186522435587,5.32758429305789,2.94565042609802));
#7361=CARTESIAN_POINT('Ctrl Pts',(1.38833450715645,3.16495931797173,1.0447803202184));
#7362=CARTESIAN_POINT('Ctrl Pts',(1.51480378995702,3.57690019914092,-1.80488441711536));
#7363=CARTESIAN_POINT('Ctrl Pts',(1.64127307275759,6.18931341035722,-3.01548925232429));
#7364=CARTESIAN_POINT('Ctrl Pts',(1.76774235555816,8.62980687076538,-1.48766065606638));
#7365=CARTESIAN_POINT('Ctrl Pts',(1.89421163835874,8.68211232342893,1.39114751979702));
#7366=CARTESIAN_POINT('Ctrl Pts',(2.02068092115931,6.29873006674212,3.00662229441761));
#7367=CARTESIAN_POINT('Ctrl Pts',(2.14715020395988,3.6440641683139,1.89171460246179));
#7368=CARTESIAN_POINT('Ctrl Pts',(2.27361948676046,3.12887765854667,-0.941102636765302));
#7369=CARTESIAN_POINT('Ctrl Pts',(2.40008876956103,5.221023215509,-2.91928291965494));
#7370=CARTESIAN_POINT('Ctrl Pts',(2.5265580523616,8.02057546463636,-2.24639543728625));
#7371=CARTESIAN_POINT('Ctrl Pts',(2.65302733516218,8.98519677504537,0.466495297308555));
#7372=CARTESIAN_POINT('Ctrl Pts',(2.77949661796275,7.23889240500353,2.75575094100713));
#7373=CARTESIAN_POINT('Ctrl Pts',(2.90596590076332,4.36752141768572,2.5424459342591));
#7374=CARTESIAN_POINT('Ctrl Pts',(3.0324351835639,2.97864168519721,0.0202874407439004));
#7375=CARTESIAN_POINT('Ctrl Pts',(3.15890446636446,4.33352675754921,-2.52029454194393));
#7376=CARTESIAN_POINT('Ctrl Pts',(3.28537374916504,7.20177441543159,-2.77213922842707));
#7377=CARTESIAN_POINT('Ctrl Pts',(3.41184303196561,8.97866315423926,-0.506540679845794));
#7378=CARTESIAN_POINT('Ctrl Pts',(3.53831231476619,8.05055954300406,2.21905908152931));
#7379=CARTESIAN_POINT('Ctrl Pts',(3.66478159756676,5.26029576462132,2.92948037902181));
#7380=CARTESIAN_POINT('Ctrl Pts',(3.79125088036734,3.14177437347817,0.979573332991449));
#7381=CARTESIAN_POINT('Ctrl Pts',(3.9177201631679,3.61887325026032,-1.85990673112716));
#7382=CARTESIAN_POINT('Ctrl Pts',(4.04418944596849,6.25832795884948,-3.01036282074418));
#7383=CARTESIAN_POINT('Ctrl Pts',(4.17065872876905,8.66318912116946,-1.42703936585924));
#7384=CARTESIAN_POINT('Ctrl Pts',(4.29712801156963,8.64954714081024,1.45221127782889));
#7385=CARTESIAN_POINT('Ctrl Pts',(4.42359729437019,6.22979061312465,3.01267554193145));
#7386=CARTESIAN_POINT('Ctrl Pts',(4.55006657717078,3.60135595755754,1.83726002636678));
#7387=CARTESIAN_POINT('Ctrl Pts',(4.67653585997134,3.1511849892005,-1.00661347153406));
#7388=CARTESIAN_POINT('Ctrl Pts',(4.80300514277192,5.28808829272449,-2.93635818112757));
#7389=CARTESIAN_POINT('Ctrl Pts',(4.92947442557249,8.07149495106845,-2.19952865735556));
#7390=CARTESIAN_POINT('Ctrl Pts',(5.05594370837307,8.9737295178849,0.534743304110009));
#7391=CARTESIAN_POINT('Ctrl Pts',(5.18241299117364,7.17545208301331,2.78340260245806));
#7392=CARTESIAN_POINT('Ctrl Pts',(5.30888227397421,4.30971964307301,2.50439013770165));
#7393=CARTESIAN_POINT('Ctrl Pts',(5.43535155677478,2.97896957548569,-0.0489164695102037));
#7394=CARTESIAN_POINT('Ctrl Pts',(5.56182083957536,4.39168654812479,-2.55780090846567));
#7395=CARTESIAN_POINT('Ctrl Pts',(5.68829012237593,7.26494986606656,-2.74388765862757));
#7396=CARTESIAN_POINT('Ctrl Pts',(5.81475940517651,8.98948318879469,-0.438187072771831));
#7397=CARTESIAN_POINT('Ctrl Pts',(5.94122868797707,7.99919823984401,2.26544124722655));
#7398=CARTESIAN_POINT('Ctrl Pts',(6.06769797077765,5.19339550153742,2.91177039443194));
#7399=CARTESIAN_POINT('Ctrl Pts',(6.19416725357823,3.12008881427174,0.913854041489789));
#7400=CARTESIAN_POINT('Ctrl Pts',(6.32063653637879,3.66209554878131,-1.91395413315054));
#7401=CARTESIAN_POINT('Ctrl Pts',(6.44710581917937,6.32720695415856,-3.00365664748478));
#7402=CARTESIAN_POINT('Ctrl Pts',(6.57357510197995,8.69517421732942,-1.3656696471219));
#7403=CARTESIAN_POINT('Ctrl Pts',(6.70004438478051,8.61559193816459,1.51251329245416));
#7404=CARTESIAN_POINT('Ctrl Pts',(6.8265136675811,6.16073061022695,3.01714820944448));
#7405=CARTESIAN_POINT('Ctrl Pts',(6.95298295038165,3.55990612749904,1.78184161478998));
#7406=CARTESIAN_POINT('Ctrl Pts',(7.07945223318224,3.17498687362254,-1.07159623119251));
#7407=CARTESIAN_POINT('Ctrl Pts',(7.2059215159828,5.35552685433585,-2.95189295389255));
#7408=CARTESIAN_POINT('Ctrl Pts',(7.33239079878339,8.12132768474379,-2.15150795971123));
#7409=CARTESIAN_POINT('Ctrl Pts',(7.45886008158395,8.96070217500711,0.602710774981116));
#7410=CARTESIAN_POINT('Ctrl Pts',(7.58532936438453,7.11139509225075,2.80959402670167));
#7411=CARTESIAN_POINT('Ctrl Pts',(7.71179864718509,4.25280462794925,2.46502048238232));
#7412=CARTESIAN_POINT('Ctrl Pts',(7.83826792998568,2.98088236599169,-0.118094717771357));
#7413=CARTESIAN_POINT('Ctrl Pts',(7.96473721278624,4.45069009732305,-2.59396539404523));
#7414=CARTESIAN_POINT('Ctrl Pts',(8.09120649558682,7.32746169336768,-2.71419658477305));
#7415=CARTESIAN_POINT('Ctrl Pts',(8.2176757783874,8.99873487696146,-0.369603580401957));
#7416=CARTESIAN_POINT('Ctrl Pts',(8.34414506118796,7.9467881045264,2.31063490665217));
#7417=CARTESIAN_POINT('Ctrl Pts',(8.47061434398854,5.12691841598226,2.89253283821776));
#7418=CARTESIAN_POINT('Ctrl Pts',(8.59708362678912,3.09991409354922,0.847655304587422));
#7419=CARTESIAN_POINT('Ctrl Pts',(8.72355290958968,3.70654441823305,-1.96699739921706));
#7420=CARTESIAN_POINT('Ctrl Pts',(8.85002219239026,6.39591418697016,-2.99537475015773));
#7421=CARTESIAN_POINT('Ctrl Pts',(8.97649147519083,8.72574556011418,-1.30358334856292));
#7422=CARTESIAN_POINT('Ctrl Pts',(9.1029607579914,8.58026416208568,1.57202158130248));
#7423=CARTESIAN_POINT('Ctrl Pts',(9.22943004079197,6.09158700182589,3.02003844763038));
#7424=CARTESIAN_POINT('Ctrl Pts',(9.35589932359257,3.51973505278771,1.72548757686079));
#7425=CARTESIAN_POINT('Ctrl Pts',(9.48236860639312,3.20027345136559,-1.1360152149446));
#7426=CARTESIAN_POINT('Ctrl Pts',(9.6088378891937,5.42329849222802,-2.96588214441775));
#7427=CARTESIAN_POINT('Ctrl Pts',(9.73530717199428,8.17005714643252,-2.10235270013504));
#7428=CARTESIAN_POINT('Ctrl Pts',(9.86177645479484,8.94610316147124,0.670350888189973));
#7429=CARTESIAN_POINT('Ctrl Pts',(9.98824573759542,7.04679029023846,2.83433283661117));
#7430=CARTESIAN_POINT('Ctrl Pts',(10.114715020396,4.19673876478062,2.42431673808699));
#7431=CARTESIAN_POINT('Ctrl Pts',(10.2411843031966,2.98450817703985,-0.187132765170506));
#7432=CARTESIAN_POINT('Ctrl Pts',(10.3676535859971,4.51025928781023,-2.62891879005706));
#7433=CARTESIAN_POINT('Ctrl Pts',(10.4941228687977,7.38975050690281,-2.68279483089907));
#7434=CARTESIAN_POINT('Ctrl Pts',(10.6205921515983,9.0055039557413,-0.301376148205788));
#7435=CARTESIAN_POINT('Ctrl Pts',(10.7470614343989,7.895127566208,2.35567940107123));
#7436=CARTESIAN_POINT('Ctrl Pts',(10.8735307171994,5.05723750909054,2.86964862298535));
#7437=CARTESIAN_POINT('Ctrl Pts',(10.9578435723998,3.7461035332853,1.48053551427594));
#7438=CARTESIAN_POINT('Ctrl Pts',(11.,3.52700509758159,0.661737268568548));
#7439=CARTESIAN_POINT('Ctrl Pts',(-2.77555756156289E-16,4.38007430561128,
1.36291222925734));
#7440=CARTESIAN_POINT('Ctrl Pts',(-2.80031029468505E-16,4.32659445095465,
1.31130786139469));
#7441=CARTESIAN_POINT('Ctrl Pts',(1.11194639968977E-16,4.27624355628285,
1.25685426489337));
#7442=CARTESIAN_POINT('Ctrl Pts',(4.68375338513738E-17,4.22901660607647,
1.19991824488684));
#7443=CARTESIAN_POINT('Ctrl Pts',(-1.93070425417206E-17,4.18047796280637,
1.14140086969662));
#7444=CARTESIAN_POINT('Ctrl Pts',(-1.48725298511017E-16,4.13523875300555,
1.08026078916569));
#7445=CARTESIAN_POINT('Ctrl Pts',(-1.66533453693773E-16,4.09332060715764,
1.01684861703025));
#7446=CARTESIAN_POINT('Ctrl Pts',(-1.8377727982304E-16,4.05273082055456,
0.955445936092179));
#7447=CARTESIAN_POINT('Ctrl Pts',(-3.01042658861766E-16,4.01525479286761,
0.891912050008348));
#7448=CARTESIAN_POINT('Ctrl Pts',(-3.33066907387547E-16,3.98094125132206,
0.826531654328836));
#7449=CARTESIAN_POINT('Ctrl Pts',(-3.47077516117576E-16,3.96592907689589,
0.79792773121905));
#7450=CARTESIAN_POINT('Ctrl Pts',(-1.42842800960507E-16,3.95152261862076,
0.768970004663094));
#7451=CARTESIAN_POINT('Ctrl Pts',(-1.45716771982052E-16,3.9377279101113,
0.739680798967653));
#7452=CARTESIAN_POINT('Ctrl Pts',(-1.47637449172231E-16,3.9285088951036,
0.720106798786031));
#7453=CARTESIAN_POINT('Ctrl Pts',(-1.72992178300136E-16,3.91956312859518,
0.700384733783148));
#7454=CARTESIAN_POINT('Ctrl Pts',(-1.73472347597681E-16,3.91089273167378,
0.680521086833724));
#7455=CARTESIAN_POINT('Ctrl Pts',(-1.73770300656856E-16,3.90551260574693,
0.668195362541848));
#7456=CARTESIAN_POINT('Ctrl Pts',(2.06740054808053E-16,3.90024214212162,
0.655823365037683));
#7457=CARTESIAN_POINT('Ctrl Pts',(2.0122792321331E-16,3.89508319856995,
0.643411203636316));
#7458=CARTESIAN_POINT('Ctrl Pts',(1.68366422301827E-16,3.86432728766482,
0.569414012859255));
#7459=CARTESIAN_POINT('Ctrl Pts',(-4.84275148589556E-16,3.83751112678279,
0.493944650744559));
#7460=CARTESIAN_POINT('Ctrl Pts',(-3.60822483003176E-16,3.81465926753848,
0.417382612231489));
#7461=CARTESIAN_POINT('Ctrl Pts',(-2.35429102250813E-16,3.79144816979904,
0.339616994123154));
#7462=CARTESIAN_POINT('Ctrl Pts',(-1.12344122363624E-16,3.77232649682797,
0.260723255358029));
#7463=CARTESIAN_POINT('Ctrl Pts',(-5.55111512312578E-17,3.75736079522538,
0.181064368578248));
#7464=CARTESIAN_POINT('Ctrl Pts',(-4.96349244774822E-18,3.74405019113428,
0.11021517403868));
#7465=CARTESIAN_POINT('Ctrl Pts',(-2.69294374879976E-16,3.73402751903509,
0.0387597845660613));
#7466=CARTESIAN_POINT('Ctrl Pts',(-2.63677968348475E-16,3.72737085088334,
-0.0330606627948158));
#7467=CARTESIAN_POINT('Ctrl Pts',(-2.6150366267442E-16,3.72479382387301,
-0.0608648477899769));
#7468=CARTESIAN_POINT('Ctrl Pts',(8.93900777674783E-17,3.7227216032029,
-0.0887238419963498));
#7469=CARTESIAN_POINT('Ctrl Pts',(1.38777878078145E-16,3.72116002426916,
-0.116623918592605));
#7470=CARTESIAN_POINT('Ctrl Pts',(1.66233930557089E-16,3.72029189908672,
-0.132134347532035));
#7471=CARTESIAN_POINT('Ctrl Pts',(2.59188299389654E-16,3.71958160408319,
-0.147657474843062));
#7472=CARTESIAN_POINT('Ctrl Pts',(2.63677968348475E-16,3.71903024499337,
-0.163190949016707));
#7473=CARTESIAN_POINT('Ctrl Pts',(2.67507061918538E-16,3.71856000864298,
-0.17643894717082));
#7474=CARTESIAN_POINT('Ctrl Pts',(-1.23245947320793E-16,3.71820570920862,
-0.189685934650389));
#7475=CARTESIAN_POINT('Ctrl Pts',(-1.11022302462516E-16,3.71796762862309,
-0.20292615382453));
#7476=CARTESIAN_POINT('Ctrl Pts',(-3.40061438085201E-17,3.71646758077648,
-0.286347329124692));
#7477=CARTESIAN_POINT('Ctrl Pts',(9.27905525951754E-17,3.71957542118597,
-0.369551234359023));
#7478=CARTESIAN_POINT('Ctrl Pts',(0.,3.72735027744889,-0.45215857472717));
#7479=CARTESIAN_POINT('Ctrl Pts',(-8.48558343440982E-17,3.73446028915422,
-0.527701985061926));
#7480=CARTESIAN_POINT('Ctrl Pts',(-2.70767289408761E-16,3.74547354769541,
-0.60274741009298));
#7481=CARTESIAN_POINT('Ctrl Pts',(-2.77555756156289E-16,3.76047169010912,
-0.677016215888271));
#7482=CARTESIAN_POINT('Ctrl Pts',(-2.865998411998E-16,3.77645697580371,
-0.756173223875352));
#7483=CARTESIAN_POINT('Ctrl Pts',(-1.65629045189422E-16,3.79696805372881,
-0.834448848484121));
#7484=CARTESIAN_POINT('Ctrl Pts',(-1.66533453693773E-16,3.82173963045682,
-0.911614883986038));
#7485=CARTESIAN_POINT('Ctrl Pts',(-1.6687918879021E-16,3.83120924891766,
-0.94111372947183));
#7486=CARTESIAN_POINT('Ctrl Pts',(-4.07690256823517E-16,3.84130202564309,
-0.970450366187668));
#7487=CARTESIAN_POINT('Ctrl Pts',(-4.16333634234434E-16,3.85200508769203,
-0.999611703631864));
#7488=CARTESIAN_POINT('Ctrl Pts',(-4.20262745966492E-16,3.8568704921128,
-1.0128678820477));
#7489=CARTESIAN_POINT('Ctrl Pts',(-5.1383979233867E-16,3.86186202208545,
-1.02608783230357));
#7490=CARTESIAN_POINT('Ctrl Pts',(-5.27355936696949E-16,3.86697853716836,
-1.03927030385677));
#7491=CARTESIAN_POINT('Ctrl Pts',(-5.3932641475938E-16,3.87150994271808,
-1.0509452669493));
#7492=CARTESIAN_POINT('Ctrl Pts',(1.87412194500338E-16,3.87613799774593,
-1.06258713958298));
#7493=CARTESIAN_POINT('Ctrl Pts',(1.66533453693773E-16,3.88085844924797,
-1.07418734184327));
#7494=CARTESIAN_POINT('Ctrl Pts',(2.64154277135885E-17,3.91253757934153,
-1.15203674170612));
#7495=CARTESIAN_POINT('Ctrl Pts',(1.31044853828581E-16,3.9484137341162,
-1.22811404869558));
#7496=CARTESIAN_POINT('Ctrl Pts',(-2.77555756156289E-17,3.98814410668546,
-1.3021798603163));
#7497=CARTESIAN_POINT('Ctrl Pts',(-1.88358197049143E-16,4.0283253707254,
-1.37708622893583));
#7498=CARTESIAN_POINT('Ctrl Pts',(-5.21101545420775E-16,4.07244924500996,
-1.44993596567706));
#7499=CARTESIAN_POINT('Ctrl Pts',(-5.55111512312578E-16,4.12021737446078,
-1.5204760132583));
#7500=CARTESIAN_POINT('Ctrl Pts',(-5.89453236598535E-16,4.16845146820379,
-1.59170415860933));
#7501=CARTESIAN_POINT('Ctrl Pts',(-9.73015521435432E-17,4.22040173027164,
-1.66057819124318));
#7502=CARTESIAN_POINT('Ctrl Pts',(0.,4.27581129957554,-1.72681968984969));
#7503=CARTESIAN_POINT('Ctrl Pts',(3.97348772770828E-17,4.29843881566099,
-1.75387062336303));
#7504=CARTESIAN_POINT('Ctrl Pts',(-1.6663043826359E-16,4.32164376063082,
-1.78048226411648));
#7505=CARTESIAN_POINT('Ctrl Pts',(-1.94289029309402E-16,4.34541073537425,
-1.8066342869413));
#7506=CARTESIAN_POINT('Ctrl Pts',(-2.11417038683516E-16,4.36012880129184,
-1.82282933069294));
#7507=CARTESIAN_POINT('Ctrl Pts',(-6.39101957865414E-16,4.37506710170624,
-1.83885279980293));
#7508=CARTESIAN_POINT('Ctrl Pts',(-6.38378239159465E-16,4.39019735919426,
-1.85467428809663));
#7509=CARTESIAN_POINT('Ctrl Pts',(-6.35371199708122E-16,4.45306333295106,
-1.92041231460757));
#7510=CARTESIAN_POINT('Ctrl Pts',(-2.58129078341152E-16,4.51929547534557,
-1.98273176066174));
#7511=CARTESIAN_POINT('Ctrl Pts',(-2.22044604925031E-16,4.58856873157643,
-2.04132864721816));
#7512=CARTESIAN_POINT('Ctrl Pts',(-1.94981249862941E-16,4.64052367374958,
-2.08527631213548));
#7513=CARTESIAN_POINT('Ctrl Pts',(-4.23851232862792E-16,4.69419050378083,
-2.12712976418203));
#7514=CARTESIAN_POINT('Ctrl Pts',(-4.16333634234434E-16,4.74945005246149,
-2.16674908321904));
#7515=CARTESIAN_POINT('Ctrl Pts',(-4.13731776004568E-16,4.7685755097546,
-2.18046142094738));
#7516=CARTESIAN_POINT('Ctrl Pts',(-2.52486346214463E-16,4.78789187530008,
-2.19390603143607));
#7517=CARTESIAN_POINT('Ctrl Pts',(-2.22044604925031E-16,4.80739457519056,
-2.20707674403954));
#7518=CARTESIAN_POINT('Ctrl Pts',(-1.97425656185765E-16,4.82316686509724,
-2.21772820761258));
#7519=CARTESIAN_POINT('Ctrl Pts',(-3.9339803241751E-16,4.83905374993306,
-2.22819555975246));
#7520=CARTESIAN_POINT('Ctrl Pts',(-4.16333634234434E-16,4.85504755554653,
-2.23847288314367));
#7521=CARTESIAN_POINT('Ctrl Pts',(-5.23613684113935E-16,4.92985772524132,
-2.28654451321636));
#7522=CARTESIAN_POINT('Ctrl Pts',(-8.0505927221409E-17,5.00703712827284,
-2.33048359411215));
#7523=CARTESIAN_POINT('Ctrl Pts',(1.66533453693773E-16,5.08631071040055,
-2.36999470778006));
#7524=CARTESIAN_POINT('Ctrl Pts',(3.67447598235833E-16,5.15078295720981,
-2.40212861927662));
#7525=CARTESIAN_POINT('Ctrl Pts',(6.09938800167838E-17,5.21664131547317,
-2.43133339556246));
#7526=CARTESIAN_POINT('Ctrl Pts',(1.11022302462516E-16,5.28375444250491,
-2.45743079686607));
#7527=CARTESIAN_POINT('Ctrl Pts',(1.24376244097105E-16,5.30138663960587,
-2.46428719804956));
#7528=CARTESIAN_POINT('Ctrl Pts',(-7.67588771122088E-18,5.31910551399007,
-2.47092900830453));
#7529=CARTESIAN_POINT('Ctrl Pts',(0.,5.33690753016716,-2.47735729053333));
#7530=CARTESIAN_POINT('Ctrl Pts',(1.2890562790225,8.11784406625472,-0.00180833638339553));
#7531=CARTESIAN_POINT('Ctrl Pts',(1.28093512868358,8.11906067093066,-0.136660465564393));
#7532=CARTESIAN_POINT('Ctrl Pts',(1.27281397834465,8.10727342448819,-0.271300590561459));
#7533=CARTESIAN_POINT('Ctrl Pts',(1.26469282800573,8.0817079134367,-0.403271335301992));
#7534=CARTESIAN_POINT('Ctrl Pts',(1.22253640040554,7.94899880564707,-1.0883239342341));
#7535=CARTESIAN_POINT('Ctrl Pts',(1.18037997280535,7.44502212184727,-1.70144771154639));
#7536=CARTESIAN_POINT('Ctrl Pts',(1.13822354520516,6.79861529368678,-1.9642626944474));
#7537=CARTESIAN_POINT('Ctrl Pts',(1.09606711760497,6.15220846552629,-2.2270776773484));
#7538=CARTESIAN_POINT('Ctrl Pts',(1.05391069000478,5.36337149300511,-2.13958386583811));
#7539=CARTESIAN_POINT('Ctrl Pts',(1.01175426240458,4.790282868037,-1.7414783762589));
#7540=CARTESIAN_POINT('Ctrl Pts',(0.969597834804393,4.21719424306888,-1.34337288667968));
#7541=CARTESIAN_POINT('Ctrl Pts',(0.927441407204202,3.85985396565383,-0.634655719031535));
#7542=CARTESIAN_POINT('Ctrl Pts',(0.885284979604011,3.88052028647255,0.0628136850736727));
#7543=CARTESIAN_POINT('Ctrl Pts',(0.84312855200382,3.90118660729128,0.76028308917888));
#7544=CARTESIAN_POINT('Ctrl Pts',(0.800972124403629,4.29985952634379,1.44650472974115));
#7545=CARTESIAN_POINT('Ctrl Pts',(0.758815696803438,4.89550975959257,1.81000334710386));
#7546=CARTESIAN_POINT('Ctrl Pts',(0.716659269203247,5.49115999284134,2.17350196446658));
#7547=CARTESIAN_POINT('Ctrl Pts',(0.674502841603056,6.28378754028639,2.21427755862973));
#7548=CARTESIAN_POINT('Ctrl Pts',(0.632346414002865,6.91350470727655,1.91360195247884));
#7549=CARTESIAN_POINT('Ctrl Pts',(0.590189986402674,7.5432218742667,1.61292634632796));
#7550=CARTESIAN_POINT('Ctrl Pts',(0.548033558802482,8.01002866080195,0.970799539863048));
#7551=CARTESIAN_POINT('Ctrl Pts',(0.505877131202291,8.10193924842326,0.279195874812881));
#7552=CARTESIAN_POINT('Ctrl Pts',(0.500270180475694,8.11416367457561,0.187210194502225));
#7553=CARTESIAN_POINT('Ctrl Pts',(0.494663229749096,8.11975621683434,0.094349272504648));
#7554=CARTESIAN_POINT('Ctrl Pts',(0.489056279022499,8.11901932033641,0.00140296810865748));
#7555=CARTESIAN_POINT('Ctrl Pts',(0.,6.66173726856851,-2.47299490241842));
#7556=CARTESIAN_POINT('Ctrl Pts',(0.042156427600191,7.4805355142759,-2.25389646671472));
#7557=CARTESIAN_POINT('Ctrl Pts',(0.126469282800573,8.86964786268114,-0.942757917500329));
#7558=CARTESIAN_POINT('Ctrl Pts',(0.252938565601146,8.35568007480496,1.89512494763008));
#7559=CARTESIAN_POINT('Ctrl Pts',(0.379407848401719,5.69862372086684,3.00550592532682));
#7560=CARTESIAN_POINT('Ctrl Pts',(0.505877131202292,3.31720488565003,1.38974961778526));
#7561=CARTESIAN_POINT('Ctrl Pts',(0.632346414002866,3.37108102552373,-1.4897402431435));
#7562=CARTESIAN_POINT('Ctrl Pts',(0.758815696803437,5.81286715979806,-3.01549246530217));
#7563=CARTESIAN_POINT('Ctrl Pts',(0.885284979604013,8.42431700898103,-1.80326119610285));
#7564=CARTESIAN_POINT('Ctrl Pts',(1.01175426240458,8.83433307398675,1.04679026852714));
#7565=CARTESIAN_POINT('Ctrl Pts',(1.13822354520516,6.67035096999308,2.94610350710691));
#7566=CARTESIAN_POINT('Ctrl Pts',(1.26469282800573,3.89764709051462,2.17005731163833));
#7567=CARTESIAN_POINT('Ctrl Pts',(1.39116211080631,3.0341175837159,-0.576701540113256));
#7568=CARTESIAN_POINT('Ctrl Pts',(1.51763139360688,4.8639846740404,-2.79972682418719));
#7569=CARTESIAN_POINT('Ctrl Pts',(1.64410067640745,7.72548774157445,-2.48026517361596));
#7570=CARTESIAN_POINT('Ctrl Pts',(1.77056995920802,9.02003873021916,0.0915870066384873));
#7571=CARTESIAN_POINT('Ctrl Pts',(1.89703924200859,7.57202172994746,2.58026440683785));
#7572=CARTESIAN_POINT('Ctrl Pts',(2.02350852480917,4.69641652838636,2.72574581528328));
#7573=CARTESIAN_POINT('Ctrl Pts',(2.14997780760974,3.00462496841716,0.395914224840739));
#7574=CARTESIAN_POINT('Ctrl Pts',(2.27644709041032,4.03300241565958,-2.29345579779455));
#7575=CARTESIAN_POINT('Ctrl Pts',(2.40291637321088,6.8476553843829,-2.90008617898366));
#7576=CARTESIAN_POINT('Ctrl Pts',(2.52938565601147,8.89253311018671,-0.873081666227454));
#7577=CARTESIAN_POINT('Ctrl Pts',(2.65585493881203,8.31063512397009,1.94678828765999));
#7578=CARTESIAN_POINT('Ctrl Pts',(2.78232422161261,5.63039638482652,2.99873515893208));
#7579=CARTESIAN_POINT('Ctrl Pts',(2.90879350441318,3.28580315999094,1.32746181821946));
#7580=CARTESIAN_POINT('Ctrl Pts',(3.03526278721375,3.4060343620134,-1.54931004838359));
#7581=CARTESIAN_POINT('Ctrl Pts',(3.16173207001433,5.88190527112525,-3.01911791792189));
#7582=CARTESIAN_POINT('Ctrl Pts',(3.2882013528149,8.46502071419216,-1.74719553636016));
#7583=CARTESIAN_POINT('Ctrl Pts',(3.41467063561548,8.80959429091728,1.11139519676803));
#7584=CARTESIAN_POINT('Ctrl Pts',(3.54113991841604,6.60271083165986,2.96070245343145));
#7585=CARTESIAN_POINT('Ctrl Pts',(3.66760920121663,3.84849183796069,2.12132788423443));
#7586=CARTESIAN_POINT('Ctrl Pts',(3.79407848401719,3.0481067685106,-0.644473206270731));
#7587=CARTESIAN_POINT('Ctrl Pts',(3.92054776681777,4.92840366803431,-2.82501339204223));
#7588=CARTESIAN_POINT('Ctrl Pts',(4.04701704961833,7.78184178235469,-2.4400941019681));
#7589=CARTESIAN_POINT('Ctrl Pts',(4.17348633241892,9.01714849317786,0.160730625342051));
#7590=CARTESIAN_POINT('Ctrl Pts',(4.29995561521948,7.51251343469132,2.61559218413545));
#7591=CARTESIAN_POINT('Ctrl Pts',(4.42642489802006,4.63433022445025,2.69517447078429));
#7592=CARTESIAN_POINT('Ctrl Pts',(4.55289418082063,2.99634307005063,0.327206984929225));
#7593=CARTESIAN_POINT('Ctrl Pts',(4.6793634636212,4.08604568686072,-2.33790467107576));
#7594=CARTESIAN_POINT('Ctrl Pts',(4.80583274642178,6.91385412742878,-2.87991145655582));
#7595=CARTESIAN_POINT('Ctrl Pts',(4.93230202922234,8.91177066825553,-0.806604574315915));
#7596=CARTESIAN_POINT('Ctrl Pts',(5.05877131202293,8.26544146026922,1.99919842784905));
#7597=CARTESIAN_POINT('Ctrl Pts',(5.18524059482349,5.56181288602103,2.98948346992642));
#7598=CARTESIAN_POINT('Ctrl Pts',(5.31170987762408,3.2561120833366,1.26494998502281));
#7599=CARTESIAN_POINT('Ctrl Pts',(5.43817916042463,3.44219885099807,-1.60831360312132));
#7600=CARTESIAN_POINT('Ctrl Pts',(5.56464844322522,5.9510835258896,-3.02103070861275));
#7601=CARTESIAN_POINT('Ctrl Pts',(5.69111772602578,8.50439037321506,-1.69028051588142));
#7602=CARTESIAN_POINT('Ctrl Pts',(5.81758700882636,8.78340286420995,1.17545219355302));
#7603=CARTESIAN_POINT('Ctrl Pts',(5.94405629162693,6.53474335439746,2.97372979753514));
#7604=CARTESIAN_POINT('Ctrl Pts',(6.07052557442751,3.80047113580028,2.07149514587238));
#7605=CARTESIAN_POINT('Ctrl Pts',(6.19699485722809,3.06364154273657,-0.711911774223792));
#7606=CARTESIAN_POINT('Ctrl Pts',(6.32346414002865,4.99338643380372,-2.84881527870274));
#7607=CARTESIAN_POINT('Ctrl Pts',(6.44993342282923,7.83726019914311,-2.39864426801156));
#7608=CARTESIAN_POINT('Ctrl Pts',(6.5764027056298,9.01267582524419,0.229790634734156));
#7609=CARTESIAN_POINT('Ctrl Pts',(6.70287198843037,7.45221141439524,2.64954738997428));
#7610=CARTESIAN_POINT('Ctrl Pts',(6.82934127123096,4.57296049994168,2.66318937161644));
#7611=CARTESIAN_POINT('Ctrl Pts',(6.95581055403151,2.9896368961606,0.258327983142764));
#7612=CARTESIAN_POINT('Ctrl Pts',(7.0822798368321,4.14009309396666,-2.38112697366136));
#7613=CARTESIAN_POINT('Ctrl Pts',(7.20874911963266,6.97957342511075,-2.8582258953101));
#7614=CARTESIAN_POINT('Ctrl Pts',(7.33521840243324,8.92948065451071,-0.739704304940699));
#7615=CARTESIAN_POINT('Ctrl Pts',(7.46168768523381,8.21905929021046,2.05055973583909));
#7616=CARTESIAN_POINT('Ctrl Pts',(7.58815696803438,5.49345927251859,2.97866343435355));
#7617=CARTESIAN_POINT('Ctrl Pts',(7.71462625083496,3.22786051088117,1.20177452844665));
#7618=CARTESIAN_POINT('Ctrl Pts',(7.84109553363553,3.47970522104534,-1.66647339916602));
#7619=CARTESIAN_POINT('Ctrl Pts',(7.96756481643612,6.02028744265461,-3.02135859893257));
#7620=CARTESIAN_POINT('Ctrl Pts',(8.09403409923666,8.54244617334588,-1.63247873583206));
#7621=CARTESIAN_POINT('Ctrl Pts',(8.22050338203726,8.75575120016859,1.23889252150743));
#7622=CARTESIAN_POINT('Ctrl Pts',(8.34697266483782,6.46649534115966,2.98519705577739));
#7623=CARTESIAN_POINT('Ctrl Pts',(8.4734419476384,3.75360435149572,2.02057565464541));
#7624=CARTESIAN_POINT('Ctrl Pts',(8.59991123043897,3.08071680575365,-0.778976857734081));
#7625=CARTESIAN_POINT('Ctrl Pts',(8.72638051323954,5.05889727484518,-2.87112261147709));
#7626=CARTESIAN_POINT('Ctrl Pts',(8.85284979604013,7.89171478015486,-2.35593605319605));
#7627=CARTESIAN_POINT('Ctrl Pts',(8.97931907884068,9.00662257753226,0.298730094753956));
#7628=CARTESIAN_POINT('Ctrl Pts',(9.10578836164127,7.39114764994812,2.68211257580753));
#7629=CARTESIAN_POINT('Ctrl Pts',(9.23225764444183,4.51233920524947,2.62980711778656));
#7630=CARTESIAN_POINT('Ctrl Pts',(9.35872692724241,2.98451046190918,0.189313428699894));
#7631=CARTESIAN_POINT('Ctrl Pts',(9.48519621004298,4.19511541707917,-2.42310002974361));
#7632=CARTESIAN_POINT('Ctrl Pts',(9.61166549284355,7.04478041145962,-2.83504094672479));
#7633=CARTESIAN_POINT('Ctrl Pts',(9.73813477564413,8.94565071555854,-0.672415773772391));
#7634=CARTESIAN_POINT('Ctrl Pts',(9.8646040584447,8.17151879730683,2.10084489825768));
#7635=CARTESIAN_POINT('Ctrl Pts',(9.99107334124527,5.42536021041376,2.96628144383517));
#7636=CARTESIAN_POINT('Ctrl Pts',(10.1175426240458,3.20108469038192,1.13796721707783));
#7637=CARTESIAN_POINT('Ctrl Pts',(10.2440119068464,3.51849277787554,-1.72375628994429));
#7638=CARTESIAN_POINT('Ctrl Pts',(10.370481189647,6.08955924048204,-3.02010646233692));
#7639=CARTESIAN_POINT('Ctrl Pts',(10.4969504724476,8.57901781465834,-1.57381085898247));
#7640=CARTESIAN_POINT('Ctrl Pts',(10.6234197552481,8.72694165367111,1.30166438987783));
#7641=CARTESIAN_POINT('Ctrl Pts',(10.7498890380487,6.39745114979413,2.99513375481657));
#7642=CARTESIAN_POINT('Ctrl Pts',(10.8763583208493,3.70897520872018,1.96852709774085));
#7643=CARTESIAN_POINT('Ctrl Pts',(11.0028276036499,3.0972650878174,-0.845492289473616));
#7644=CARTESIAN_POINT('Ctrl Pts',(11.1292968864504,5.12911981582823,-2.89227229900937));
#7645=CARTESIAN_POINT('Ctrl Pts',(11.2136097416508,6.99952657216188,-2.50459204726911));
#7646=CARTESIAN_POINT('Ctrl Pts',(11.255766169251,7.64811304057568,-1.9589087282169));
#7647=CARTESIAN_POINT('Ctrl Pts',(-0.0852553897503347,6.62356674643624,
-2.33034688916694));
#7648=CARTESIAN_POINT('Ctrl Pts',(-0.0430989621501437,7.39513483291858,
-2.12388655333521));
#7649=CARTESIAN_POINT('Ctrl Pts',(0.0412138930502383,8.70411999768534,-0.888377480332016));
#7650=CARTESIAN_POINT('Ctrl Pts',(0.167683175850812,8.2197990496567,1.7858097976561));
#7651=CARTESIAN_POINT('Ctrl Pts',(0.294152458651384,5.71600779530122,2.83214145593622));
#7652=CARTESIAN_POINT('Ctrl Pts',(0.420621741451958,3.47195465591787,1.30958567498853));
#7653=CARTESIAN_POINT('Ctrl Pts',(0.547091024252531,3.52272309657751,-1.40380861193092));
#7654=CARTESIAN_POINT('Ctrl Pts',(0.673560307053103,5.823661410867,-2.84155194939997));
#7655=CARTESIAN_POINT('Ctrl Pts',(0.800029589853677,8.28447684817651,-1.69924495783807));
#7656=CARTESIAN_POINT('Ctrl Pts',(0.926498872654249,8.67084224693258,0.986409006944131));
#7657=CARTESIAN_POINT('Ctrl Pts',(1.05296815545482,6.6316835898229,2.77616550532978));
#7658=CARTESIAN_POINT('Ctrl Pts',(1.1794374382554,4.01891562422582,2.04488343285502));
#7659=CARTESIAN_POINT('Ctrl Pts',(1.30590672105597,3.20519647830103,-0.543436073671827));
#7660=CARTESIAN_POINT('Ctrl Pts',(1.43237600385654,4.92951264141021,-2.63823216492743));
#7661=CARTESIAN_POINT('Ctrl Pts',(1.55884528665712,7.62595765439769,-2.33719779446077));
#7662=CARTESIAN_POINT('Ctrl Pts',(1.68531456945769,8.84583597533803,0.0863040582086905));
#7663=CARTESIAN_POINT('Ctrl Pts',(1.81178385225826,7.4813439140143,2.43142884274551));
#7664=CARTESIAN_POINT('Ctrl Pts',(1.93825313505883,4.77161021040782,2.56851855015692));
#7665=CARTESIAN_POINT('Ctrl Pts',(2.06472241785941,3.17740506463998,0.37307698504849));
#7666=CARTESIAN_POINT('Ctrl Pts',(2.19119170065998,4.14646334402713,-2.16116401154155));
#7667=CARTESIAN_POINT('Ctrl Pts',(2.31766098346055,6.79876067926811,-2.73280256214906));
#7668=CARTESIAN_POINT('Ctrl Pts',(2.44413026626113,8.72568517166943,-0.822720314907301));
#7669=CARTESIAN_POINT('Ctrl Pts',(2.5705995490617,8.17735239481401,1.83449307783794));
#7670=CARTESIAN_POINT('Ctrl Pts',(2.69706883186227,5.65171596835802,2.82576124286347));
#7671=CARTESIAN_POINT('Ctrl Pts',(2.82353811466284,3.44236425375709,1.25089077844456));
#7672=CARTESIAN_POINT('Ctrl Pts',(2.95000739746342,3.55566024451705,-1.45994229429062));
#7673=CARTESIAN_POINT('Ctrl Pts',(3.07647668026399,5.88871724572051,-2.84496827760426));
#7674=CARTESIAN_POINT('Ctrl Pts',(3.20294596306456,8.32283267039175,-1.64641329383313));
#7675=CARTESIAN_POINT('Ctrl Pts',(3.32941524586514,8.6475304535636,1.04728737487113));
#7676=CARTESIAN_POINT('Ctrl Pts',(3.45588452866571,6.56794508967739,2.7899223509744));
#7677=CARTESIAN_POINT('Ctrl Pts',(3.58235381146628,3.97259575928665,1.99896483049539));
#7678=CARTESIAN_POINT('Ctrl Pts',(3.70882309426686,3.21837873485823,-0.607298514815273));
#7679=CARTESIAN_POINT('Ctrl Pts',(3.83529237706743,4.99021580020368,-2.66206014560021));
#7680=CARTESIAN_POINT('Ctrl Pts',(3.96176165986801,7.67906106496106,-2.29934388228426));
#7681=CARTESIAN_POINT('Ctrl Pts',(4.08823094266857,8.84311245379272,0.151459314531306));
#7682=CARTESIAN_POINT('Ctrl Pts',(4.21470022546915,7.42526819360171,2.46471883288909));
#7683=CARTESIAN_POINT('Ctrl Pts',(4.34116950826972,4.71310518676386,2.53971063086796));
#7684=CARTESIAN_POINT('Ctrl Pts',(4.4676387910703,3.16960088515058,0.308332936189166));
#7685=CARTESIAN_POINT('Ctrl Pts',(4.59410807387087,4.19644695778789,-2.2030489719499));
#7686=CARTESIAN_POINT('Ctrl Pts',(4.72057735667144,6.86114092710966,-2.71379156394459));
#7687=CARTESIAN_POINT('Ctrl Pts',(4.84704663947202,8.74381306330275,-0.760077774000557));
#7688=CARTESIAN_POINT('Ctrl Pts',(4.97351592227259,8.13476560520423,1.88388008103432));
#7689=CARTESIAN_POINT('Ctrl Pts',(5.09998520507317,5.58708852293413,2.81704321248145));
#7690=CARTESIAN_POINT('Ctrl Pts',(5.22645448787373,3.41438582644622,1.19198477104298));
#7691=CARTESIAN_POINT('Ctrl Pts',(5.35292377067431,3.58973868290013,-1.51554238877461));
#7692=CARTESIAN_POINT('Ctrl Pts',(5.47939305347488,5.95390514021654,-2.8467707341446));
#7693=CARTESIAN_POINT('Ctrl Pts',(5.60586233627546,8.35993139726009,-1.59278126216586));
#7694=CARTESIAN_POINT('Ctrl Pts',(5.73233161907603,8.62284980837074,1.10764941728427));
#7695=CARTESIAN_POINT('Ctrl Pts',(5.8588009018766,6.50389813226231,2.80219824801587));
#7696=CARTESIAN_POINT('Ctrl Pts',(5.98527018467718,3.92734500127429,1.95200655868209));
#7697=CARTESIAN_POINT('Ctrl Pts',(6.11173946747773,3.23301742770633,-0.670847071622082));
#7698=CARTESIAN_POINT('Ctrl Pts',(6.23820875027833,5.05145021112467,-2.68448908489215));
#7699=CARTESIAN_POINT('Ctrl Pts',(6.36467803307889,7.73128282046858,-2.26028496973954));
#7700=CARTESIAN_POINT('Ctrl Pts',(6.49114731587947,8.83889777959534,0.216535784319152));
#7701=CARTESIAN_POINT('Ctrl Pts',(6.61761659868004,7.36844453202843,2.49671542464112));
#7702=CARTESIAN_POINT('Ctrl Pts',(6.74408588148061,4.6552754086039,2.50957050551929));
#7703=CARTESIAN_POINT('Ctrl Pts',(6.87055516428119,3.16328153873884,0.243427033073461));
#7704=CARTESIAN_POINT('Ctrl Pts',(6.99702444708175,4.24737678659332,-2.24377811307125));
#7705=CARTESIAN_POINT('Ctrl Pts',(7.12349372988233,6.92306938509461,-2.6933568755676));
#7706=CARTESIAN_POINT('Ctrl Pts',(7.2499630126829,8.76050149696535,-0.697036465476021));
#7707=CARTESIAN_POINT('Ctrl Pts',(7.37643229548347,8.09105886500692,1.93227875107649));
#7708=CARTESIAN_POINT('Ctrl Pts',(7.50290157828406,5.52267770250222,2.80684730135633));
#7709=CARTESIAN_POINT('Ctrl Pts',(7.62937086108461,3.38776386943321,1.13245341957922));
#7710=CARTESIAN_POINT('Ctrl Pts',(7.75584014388521,3.62508159957098,-1.57034739450059));
#7711=CARTESIAN_POINT('Ctrl Pts',(7.88230942668576,6.01911721647024,-2.84707971099935));
#7712=CARTESIAN_POINT('Ctrl Pts',(8.00877870948634,8.39579205162815,-1.53831362125216));
#7713=CARTESIAN_POINT('Ctrl Pts',(8.13524799228692,8.5967931556797,1.16743036173818));
#7714=CARTESIAN_POINT('Ctrl Pts',(8.26171727508749,6.43958682082974,2.81300404852356));
#7715=CARTESIAN_POINT('Ctrl Pts',(8.38818655788806,3.88318160049148,1.90402422039959));
#7716=CARTESIAN_POINT('Ctrl Pts',(8.51465584068864,3.24910775042176,-0.734043687424681));
#7717=CARTESIAN_POINT('Ctrl Pts',(8.64112512348919,5.11318223672586,-2.70550967959111));
#7718=CARTESIAN_POINT('Ctrl Pts',(8.7675944062898,7.78259633645583,-2.22004026262758));
#7719=CARTESIAN_POINT('Ctrl Pts',(8.89406368909034,8.83319369708346,0.281498658298747));
#7720=CARTESIAN_POINT('Ctrl Pts',(9.02053297189094,7.31090306545242,2.52740217592696));
#7721=CARTESIAN_POINT('Ctrl Pts',(9.14700225469149,4.59815088911334,2.47811381659131));
#7722=CARTESIAN_POINT('Ctrl Pts',(9.27347153749208,3.15845080896311,0.178393396289211));
#7723=CARTESIAN_POINT('Ctrl Pts',(9.39994082029265,4.29922529601587,-2.28333006709043));
#7724=CARTESIAN_POINT('Ctrl Pts',(9.52641010309322,6.98451508303819,-2.67150928794886));
#7725=CARTESIAN_POINT('Ctrl Pts',(9.6528793858938,8.77573883183555,-0.633629290988387));
#7726=CARTESIAN_POINT('Ctrl Pts',(9.77934866869436,8.04626061668093,1.97966335008995));
#7727=CARTESIAN_POINT('Ctrl Pts',(9.90581795149495,5.45850675035994,2.79517953242645));
#7728=CARTESIAN_POINT('Ctrl Pts',(10.0322872342955,3.36253253962162,1.07232666015524));
#7729=CARTESIAN_POINT('Ctrl Pts',(10.1587565170961,3.66163180123505,-1.62432607686547));
#7730=CARTESIAN_POINT('Ctrl Pts',(10.2852257998967,6.08439325825112,-2.84589980051202));
#7731=CARTESIAN_POINT('Ctrl Pts',(10.4116950826972,8.43025415685968,-1.48302984198647));
#7732=CARTESIAN_POINT('Ctrl Pts',(10.5381643654978,8.56964540984608,1.22658140488878));
#7733=CARTESIAN_POINT('Ctrl Pts',(10.6646336482984,6.37452525664845,2.82236757599056));
#7734=CARTESIAN_POINT('Ctrl Pts',(10.791102931099,3.84112676894634,1.85497794353522));
#7735=CARTESIAN_POINT('Ctrl Pts',(10.9175722138995,3.26470148965294,-0.79672235663028));
#7736=CARTESIAN_POINT('Ctrl Pts',(11.0440414967001,5.17935418061835,-2.72543940467849));
#7737=CARTESIAN_POINT('Ctrl Pts',(11.1283543519005,6.94187158889785,-2.36012143829251));
#7738=CARTESIAN_POINT('Ctrl Pts',(11.1705107795007,7.55304610346956,-1.84591438360752));
#7739=CARTESIAN_POINT('Ctrl Pts',(-0.170510779500669,6.58539622430396,-2.18769887591546));
#7740=CARTESIAN_POINT('Ctrl Pts',(-0.128354351900478,7.30973415156126,-1.9938766399557));
#7741=CARTESIAN_POINT('Ctrl Pts',(-0.0440414967000963,8.53859213268954,
-0.833997043163702));
#7742=CARTESIAN_POINT('Ctrl Pts',(0.0824277861004767,8.08391802450845,1.67649464768213));
#7743=CARTESIAN_POINT('Ctrl Pts',(0.20889706890105,5.73339186973559,2.65877698654563));
#7744=CARTESIAN_POINT('Ctrl Pts',(0.335366351701623,3.62670442618572,1.2294217321918));
#7745=CARTESIAN_POINT('Ctrl Pts',(0.461835634502196,3.67436516763127,-1.31787698071835));
#7746=CARTESIAN_POINT('Ctrl Pts',(0.588304917302769,5.83445566193595,-2.66761143349777));
#7747=CARTESIAN_POINT('Ctrl Pts',(0.714774200103342,8.14463668737201,-1.59522871957328));
#7748=CARTESIAN_POINT('Ctrl Pts',(0.841243482903916,8.50735141987839,0.926027745361123));
#7749=CARTESIAN_POINT('Ctrl Pts',(0.967712765704488,6.59301620965272,2.60622750355264));
#7750=CARTESIAN_POINT('Ctrl Pts',(1.09418204850506,4.14018415793702,1.91970955407172));
#7751=CARTESIAN_POINT('Ctrl Pts',(1.22065133130563,3.37627537288617,-0.5101706072304));
#7752=CARTESIAN_POINT('Ctrl Pts',(1.34712061410621,4.99504060878001,-2.47673750566767));
#7753=CARTESIAN_POINT('Ctrl Pts',(1.47358989690678,7.52642756722094,-2.19413041530558));
#7754=CARTESIAN_POINT('Ctrl Pts',(1.60005917970735,8.6716332204569,0.0810211097788901));
#7755=CARTESIAN_POINT('Ctrl Pts',(1.72652846250793,7.39066609808113,2.28259327865317));
#7756=CARTESIAN_POINT('Ctrl Pts',(1.8529977453085,4.84680389242928,2.41129128503055));
#7757=CARTESIAN_POINT('Ctrl Pts',(1.97946702810908,3.3501851608628,0.350239745256248));
#7758=CARTESIAN_POINT('Ctrl Pts',(2.10593631090965,4.25992427239468,-2.02887222528856));
#7759=CARTESIAN_POINT('Ctrl Pts',(2.23240559371022,6.74986597415332,-2.56551894531445));
#7760=CARTESIAN_POINT('Ctrl Pts',(2.35887487651079,8.55883723315213,-0.772358963587151));
#7761=CARTESIAN_POINT('Ctrl Pts',(2.48534415931136,8.04406966565793,1.72219786801588));
#7762=CARTESIAN_POINT('Ctrl Pts',(2.61181344211194,5.6730355518895,2.65278732679486));
#7763=CARTESIAN_POINT('Ctrl Pts',(2.73828272491251,3.59892534752324,1.17431973866966));
#7764=CARTESIAN_POINT('Ctrl Pts',(2.86475200771308,3.7052861270207,-1.37057454019767));
#7765=CARTESIAN_POINT('Ctrl Pts',(2.99122129051366,5.89552922031577,-2.67081863728663));
#7766=CARTESIAN_POINT('Ctrl Pts',(3.11769057331423,8.18064462659133,-1.54563105130611));
#7767=CARTESIAN_POINT('Ctrl Pts',(3.24415985611481,8.48546661620991,0.983179552974222));
#7768=CARTESIAN_POINT('Ctrl Pts',(3.37062913891538,6.53317934769492,2.61914224851735));
#7769=CARTESIAN_POINT('Ctrl Pts',(3.49709842171595,4.09669968061262,1.87660177675634));
#7770=CARTESIAN_POINT('Ctrl Pts',(3.62356770451652,3.38865070120585,-0.570123823359812));
#7771=CARTESIAN_POINT('Ctrl Pts',(3.7500369873171,5.05202793237307,-2.49910689915819));
#7772=CARTESIAN_POINT('Ctrl Pts',(3.87650627011767,7.57628034756741,-2.15859366260042));
#7773=CARTESIAN_POINT('Ctrl Pts',(4.00297555291824,8.6690764144076,0.14218800372056));
#7774=CARTESIAN_POINT('Ctrl Pts',(4.12944483571882,7.33802295251209,2.31384548164274));
#7775=CARTESIAN_POINT('Ctrl Pts',(4.25591411851938,4.79188014907748,2.38424679095162));
#7776=CARTESIAN_POINT('Ctrl Pts',(4.38238340131997,3.34285870025051,0.289458887449109));
#7777=CARTESIAN_POINT('Ctrl Pts',(4.50885268412053,4.30684822871507,-2.06819327282405));
#7778=CARTESIAN_POINT('Ctrl Pts',(4.63532196692111,6.80842772679051,-2.54767167133336));
#7779=CARTESIAN_POINT('Ctrl Pts',(4.76179124972169,8.57585545835,-0.7135509736852));
#7780=CARTESIAN_POINT('Ctrl Pts',(4.88826053252225,8.00408975013921,1.76856173421959));
#7781=CARTESIAN_POINT('Ctrl Pts',(5.01472981532284,5.61236415984724,2.64460295503647));
#7782=CARTESIAN_POINT('Ctrl Pts',(5.1411990981234,3.57265956955584,1.11901955706315));
#7783=CARTESIAN_POINT('Ctrl Pts',(5.26766838092398,3.7372785148022,-1.4227711744279));
#7784=CARTESIAN_POINT('Ctrl Pts',(5.39413766372454,5.95672675454348,-2.67251075967644));
#7785=CARTESIAN_POINT('Ctrl Pts',(5.52060694652512,8.2154724213051,-1.49528200845031));
#7786=CARTESIAN_POINT('Ctrl Pts',(5.64707622932569,8.46229675253154,1.03984664101552));
#7787=CARTESIAN_POINT('Ctrl Pts',(5.77354551212627,6.47305291012714,2.63066669849658));
#7788=CARTESIAN_POINT('Ctrl Pts',(5.90001479492684,4.05421886674831,1.8325179714918));
#7789=CARTESIAN_POINT('Ctrl Pts',(6.02648407772741,3.40239331267608,-0.629782369020372));
#7790=CARTESIAN_POINT('Ctrl Pts',(6.15295336052798,5.10951398844563,-2.52016289108156));
#7791=CARTESIAN_POINT('Ctrl Pts',(6.27942264332856,7.62530544179405,-2.12192567146752));
#7792=CARTESIAN_POINT('Ctrl Pts',(6.40589192612913,8.66511973394649,0.203280933904147));
#7793=CARTESIAN_POINT('Ctrl Pts',(6.53236120892971,7.28467764966163,2.34388345930797));
#7794=CARTESIAN_POINT('Ctrl Pts',(6.65883049173027,4.73759031726612,2.35595163942215));
#7795=CARTESIAN_POINT('Ctrl Pts',(6.78529977453086,3.33692618131707,0.228526083004159));
#7796=CARTESIAN_POINT('Ctrl Pts',(6.91176905733142,4.35466047921999,-2.10642925248115));
#7797=CARTESIAN_POINT('Ctrl Pts',(7.038238340132,6.86656534507845,-2.52848785582511));
#7798=CARTESIAN_POINT('Ctrl Pts',(7.16470762293257,8.59152233942002,-0.654368626011341));
#7799=CARTESIAN_POINT('Ctrl Pts',(7.29117690573314,7.96305843980337,1.8139977663139));
#7800=CARTESIAN_POINT('Ctrl Pts',(7.41764618853372,5.55189613248584,2.63503116835912));
#7801=CARTESIAN_POINT('Ctrl Pts',(7.54411547133428,3.54766722798525,1.06313231071179));
#7802=CARTESIAN_POINT('Ctrl Pts',(7.67058475413487,3.77045797809661,-1.47422138983515));
#7803=CARTESIAN_POINT('Ctrl Pts',(7.79705403693543,6.01794699028587,-2.67280082306613));
#7804=CARTESIAN_POINT('Ctrl Pts',(7.92352331973602,8.24913792991041,-1.44414850667227));
#7805=CARTESIAN_POINT('Ctrl Pts',(8.04999260253657,8.4378351111908,1.09596820196894));
#7806=CARTESIAN_POINT('Ctrl Pts',(8.17646188533716,6.41267830049983,2.64081104126973));
#7807=CARTESIAN_POINT('Ctrl Pts',(8.30293116813773,4.01275884948723,1.78747278615377));
#7808=CARTESIAN_POINT('Ctrl Pts',(8.4294004509383,3.41749869508988,-0.689110517115282));
#7809=CARTESIAN_POINT('Ctrl Pts',(8.55586973373887,5.16746719860653,-2.53989674770512));
#7810=CARTESIAN_POINT('Ctrl Pts',(8.68233901653946,7.6734778927568,-2.08414447205911));
#7811=CARTESIAN_POINT('Ctrl Pts',(8.80880829934001,8.65976481663465,0.264267221843539));
#7812=CARTESIAN_POINT('Ctrl Pts',(8.93527758214061,7.23065848095672,2.3726917760464));
#7813=CARTESIAN_POINT('Ctrl Pts',(9.06174686494115,4.6839625729772,2.32642051539608));
#7814=CARTESIAN_POINT('Ctrl Pts',(9.18821614774176,3.33239115601705,0.167473363878527));
#7815=CARTESIAN_POINT('Ctrl Pts',(9.31468543054229,4.40333517495259,-2.14356010443725));
#7816=CARTESIAN_POINT('Ctrl Pts',(9.4411547133429,6.92424975461675,-2.50797762917294));
#7817=CARTESIAN_POINT('Ctrl Pts',(9.56762399614345,8.60582694811258,-0.594842808204379));
#7818=CARTESIAN_POINT('Ctrl Pts',(9.69409327894404,7.92100243605504,1.85848180192222));
#7819=CARTESIAN_POINT('Ctrl Pts',(9.8205625617446,5.49165329030611,2.62407762101773));
#7820=CARTESIAN_POINT('Ctrl Pts',(9.94703184454518,3.52398038886132,1.00668610323265));
#7821=CARTESIAN_POINT('Ctrl Pts',(10.0735011273458,3.80477082459457,-1.52489586378665));
#7822=CARTESIAN_POINT('Ctrl Pts',(10.1999704101463,6.0792272760202,-2.67169313868712));
#7823=CARTESIAN_POINT('Ctrl Pts',(10.3264396929469,8.28149049906102,-1.39224882499048));
#7824=CARTESIAN_POINT('Ctrl Pts',(10.4529089757474,8.41234916602104,1.15149841989973));
#7825=CARTESIAN_POINT('Ctrl Pts',(10.5793782585481,6.35159936350278,2.64960139716456));
#7826=CARTESIAN_POINT('Ctrl Pts',(10.7058475413486,3.9732783291725,1.74142878932959));
#7827=CARTESIAN_POINT('Ctrl Pts',(10.8323168241492,3.43213789148847,-0.747952423786943));
#7828=CARTESIAN_POINT('Ctrl Pts',(10.9587861069498,5.22958854540846,-2.55860651034762));
#7829=CARTESIAN_POINT('Ctrl Pts',(11.0430989621501,6.88421660563383,-2.21565082931592));
#7830=CARTESIAN_POINT('Ctrl Pts',(11.0852553897503,7.45797916636344,-1.73292003899813));
#7831=CARTESIAN_POINT('Ctrl Pts',(-0.255766169251004,6.54722570217169,-2.04505086266398));
#7832=CARTESIAN_POINT('Ctrl Pts',(-0.213609741650813,7.22433347020394,-1.8638667265762));
#7833=CARTESIAN_POINT('Ctrl Pts',(-0.129296886450431,8.37306426769373,-0.779616605995389));
#7834=CARTESIAN_POINT('Ctrl Pts',(-0.00282760364985813,7.94803699936021,
1.56717949770815));
#7835=CARTESIAN_POINT('Ctrl Pts',(0.123641679150715,5.75077594416995,2.48541251715503));
#7836=CARTESIAN_POINT('Ctrl Pts',(0.250110961951289,3.78145419645358,1.14925778939507));
#7837=CARTESIAN_POINT('Ctrl Pts',(0.376580244751861,3.82600723868504,-1.23194534950577));
#7838=CARTESIAN_POINT('Ctrl Pts',(0.503049527552435,5.84524991300489,-2.49367091759558));
#7839=CARTESIAN_POINT('Ctrl Pts',(0.629518810353007,8.00479652656751,-1.49121248130849));
#7840=CARTESIAN_POINT('Ctrl Pts',(0.755988093153581,8.3438605928242,0.86564648377811));
#7841=CARTESIAN_POINT('Ctrl Pts',(0.882457375954154,6.55434882948256,2.43628950177551));
#7842=CARTESIAN_POINT('Ctrl Pts',(1.00892665875473,4.26145269164822,1.79453567528841));
#7843=CARTESIAN_POINT('Ctrl Pts',(1.1353959415553,3.54735426747131,-0.476905140788969));
#7844=CARTESIAN_POINT('Ctrl Pts',(1.26186522435587,5.06056857614981,-2.31524284640792));
#7845=CARTESIAN_POINT('Ctrl Pts',(1.38833450715645,7.42689748004418,-2.05106303615039));
#7846=CARTESIAN_POINT('Ctrl Pts',(1.51480378995702,8.49743046557577,0.0757381613490904));
#7847=CARTESIAN_POINT('Ctrl Pts',(1.64127307275759,7.29998828214797,2.13375771456083));
#7848=CARTESIAN_POINT('Ctrl Pts',(1.76774235555816,4.92199757445075,2.25406401990418));
#7849=CARTESIAN_POINT('Ctrl Pts',(1.89421163835874,3.52296525708561,0.327402505464004));
#7850=CARTESIAN_POINT('Ctrl Pts',(2.02068092115931,4.37338520076223,-1.89658043903557));
#7851=CARTESIAN_POINT('Ctrl Pts',(2.14715020395988,6.70097126903852,-2.39823532847985));
#7852=CARTESIAN_POINT('Ctrl Pts',(2.27361948676046,8.39198929463486,-0.721997612266999));
#7853=CARTESIAN_POINT('Ctrl Pts',(2.40008876956103,7.91078693650184,1.60990265819383));
#7854=CARTESIAN_POINT('Ctrl Pts',(2.52655805236161,5.69435513542099,2.47981341072626));
#7855=CARTESIAN_POINT('Ctrl Pts',(2.65302733516217,3.75548644128939,1.09774869889476));
#7856=CARTESIAN_POINT('Ctrl Pts',(2.77949661796276,3.85491200952435,-1.28120678610471));
#7857=CARTESIAN_POINT('Ctrl Pts',(2.90596590076332,5.90234119491101,-2.496668996969));
#7858=CARTESIAN_POINT('Ctrl Pts',(3.0324351835639,8.03845658279093,-1.44484880877908));
#7859=CARTESIAN_POINT('Ctrl Pts',(3.15890446636447,8.32340277885622,0.919071731077316));
#7860=CARTESIAN_POINT('Ctrl Pts',(3.28537374916504,6.49841360571246,2.44836214606031));
#7861=CARTESIAN_POINT('Ctrl Pts',(3.41184303196562,4.22080360193859,1.7542387230173));
#7862=CARTESIAN_POINT('Ctrl Pts',(3.53831231476619,3.55892266755349,-0.532949131904351));
#7863=CARTESIAN_POINT('Ctrl Pts',(3.66478159756676,5.11384006454244,-2.33615365271617));
#7864=CARTESIAN_POINT('Ctrl Pts',(3.79125088036733,7.47349963017379,-2.01784344291659));
#7865=CARTESIAN_POINT('Ctrl Pts',(3.91772016316791,8.49504037502246,0.132916692909814));
#7866=CARTESIAN_POINT('Ctrl Pts',(4.04418944596848,7.25077771142249,2.16297213039638));
#7867=CARTESIAN_POINT('Ctrl Pts',(4.17065872876906,4.87065511139108,2.22878295103529));
#7868=CARTESIAN_POINT('Ctrl Pts',(4.29712801156962,3.51611651535046,0.27058483870905));
#7869=CARTESIAN_POINT('Ctrl Pts',(4.42359729437021,4.41724949964224,-1.93333757369819));
#7870=CARTESIAN_POINT('Ctrl Pts',(4.55006657717077,6.75571452647139,-2.38155177872214));
#7871=CARTESIAN_POINT('Ctrl Pts',(4.67653585997135,8.40789785339724,-0.667024173369842));
#7872=CARTESIAN_POINT('Ctrl Pts',(4.80300514277192,7.8734138950742,1.65324338740486));
#7873=CARTESIAN_POINT('Ctrl Pts',(4.92947442557249,5.63763979676036,2.4721626975915));
#7874=CARTESIAN_POINT('Ctrl Pts',(5.05594370837307,3.73093331266546,1.04605434308332));
#7875=CARTESIAN_POINT('Ctrl Pts',(5.18241299117363,3.88481834670426,-1.32999996008119));
#7876=CARTESIAN_POINT('Ctrl Pts',(5.30888227397422,5.95954836887043,-2.49825078520828));
#7877=CARTESIAN_POINT('Ctrl Pts',(5.43535155677478,8.07101344535011,-1.39778275473475));
#7878=CARTESIAN_POINT('Ctrl Pts',(5.56182083957536,8.30174369669236,0.972043864746774));
#7879=CARTESIAN_POINT('Ctrl Pts',(5.68829012237593,6.44220768799198,2.45913514897731));
#7880=CARTESIAN_POINT('Ctrl Pts',(5.8147594051765,4.18109273222233,1.7130293843015));
#7881=CARTESIAN_POINT('Ctrl Pts',(5.94122868797708,3.57176919764584,-0.588717666418658));
#7882=CARTESIAN_POINT('Ctrl Pts',(6.06769797077765,5.16757776576658,-2.35583669727097));
#7883=CARTESIAN_POINT('Ctrl Pts',(6.19416725357822,7.51932806311952,-1.9835663731955));
#7884=CARTESIAN_POINT('Ctrl Pts',(6.32063653637881,8.49134168829764,0.190026083489143));
#7885=CARTESIAN_POINT('Ctrl Pts',(6.44710581917936,7.20091076729482,2.19105149397482));
#7886=CARTESIAN_POINT('Ctrl Pts',(6.57357510197996,4.81990522592834,2.202332773325));
#7887=CARTESIAN_POINT('Ctrl Pts',(6.70004438478051,3.51057082389531,0.213625132934857));
#7888=CARTESIAN_POINT('Ctrl Pts',(6.82651366758109,4.46194417184665,-1.96908039189105));
#7889=CARTESIAN_POINT('Ctrl Pts',(6.95298295038166,6.81006130506229,-2.36361883608261));
#7890=CARTESIAN_POINT('Ctrl Pts',(7.07945223318223,8.42254318187467,-0.611700786546665));
#7891=CARTESIAN_POINT('Ctrl Pts',(7.20592151598281,7.83505801459984,1.69571678155131));
#7892=CARTESIAN_POINT('Ctrl Pts',(7.33239079878338,5.58111456246946,2.4632150353619));
#7893=CARTESIAN_POINT('Ctrl Pts',(7.45886008158396,3.70757058653729,0.993811201844362));
#7894=CARTESIAN_POINT('Ctrl Pts',(7.58532936438453,3.91583435662225,-1.37809538516971));
#7895=CARTESIAN_POINT('Ctrl Pts',(7.71179864718509,6.0167767641015,-2.49852193513291));
#7896=CARTESIAN_POINT('Ctrl Pts',(7.83826792998569,8.10248380819267,-1.34998339209237));
#7897=CARTESIAN_POINT('Ctrl Pts',(7.96473721278623,8.27887706670191,1.0245060421997));
#7898=CARTESIAN_POINT('Ctrl Pts',(8.09120649558683,6.38576978016992,2.46861803401591));
#7899=CARTESIAN_POINT('Ctrl Pts',(8.21767577838739,4.14233609848298,1.67092135190795));
#7900=CARTESIAN_POINT('Ctrl Pts',(8.34414506118797,3.58588963975799,-0.64417734680588));
#7901=CARTESIAN_POINT('Ctrl Pts',(8.47061434398853,5.22175216048721,-2.37428381581914));
#7902=CARTESIAN_POINT('Ctrl Pts',(8.59708362678913,7.56435944905776,-1.94824868149064));
#7903=CARTESIAN_POINT('Ctrl Pts',(8.72355290958967,8.48633593618585,0.247035785388331));
#7904=CARTESIAN_POINT('Ctrl Pts',(8.85002219239027,7.15041389646101,2.21798137616584));
#7905=CARTESIAN_POINT('Ctrl Pts',(8.97649147519083,4.76977425684107,2.17472721420083));
#7906=CARTESIAN_POINT('Ctrl Pts',(9.10296075799141,3.50633150307099,0.156553331467843));
#7907=CARTESIAN_POINT('Ctrl Pts',(9.22943004079197,4.5074450538893,-2.00379014178407));
#7908=CARTESIAN_POINT('Ctrl Pts',(9.35589932359255,6.86398442619531,-2.34444597039702));
#7909=CARTESIAN_POINT('Ctrl Pts',(9.48236860639313,8.43591506438961,-0.556056325420373));
#7910=CARTESIAN_POINT('Ctrl Pts',(9.60883788919369,7.79574425542913,1.7373002537545));
#7911=CARTESIAN_POINT('Ctrl Pts',(9.73530717199428,5.52479983025231,2.45297570960901));
#7912=CARTESIAN_POINT('Ctrl Pts',(9.86177645479484,3.68542823810099,0.941045546310063));
#7913=CARTESIAN_POINT('Ctrl Pts',(9.98824573759541,3.94790984795411,-1.42546565070784));
#7914=CARTESIAN_POINT('Ctrl Pts',(10.114715020396,6.07406129378925,-2.49748647686222));
#7915=CARTESIAN_POINT('Ctrl Pts',(10.2411843031966,8.13272684126239,-1.30146780799449));
#7916=CARTESIAN_POINT('Ctrl Pts',(10.3676535859971,8.25505292219599,1.07641543491069));
#7917=CARTESIAN_POINT('Ctrl Pts',(10.4941228687977,6.32867347035711,2.47683521833855));
#7918=CARTESIAN_POINT('Ctrl Pts',(10.6205921515983,4.10542988939866,1.62787963512397));
#7919=CARTESIAN_POINT('Ctrl Pts',(10.7470614343988,3.59957429332401,-0.69918249094361));
#7920=CARTESIAN_POINT('Ctrl Pts',(10.8735307171994,5.27982291019858,-2.39177361601674));
#7921=CARTESIAN_POINT('Ctrl Pts',(10.9578435723998,6.8265616223698,-2.07118022033933));
#7922=CARTESIAN_POINT('Ctrl Pts',(11.,7.36291222925732,-1.61992569438875));
#7923=CARTESIAN_POINT('Ctrl Pts',(0.710943720977492,8.11470858782477,0.00143578057856379));
#7924=CARTESIAN_POINT('Ctrl Pts',(0.725958511702855,8.11629544067967,0.251703656050626));
#7925=CARTESIAN_POINT('Ctrl Pts',(0.740973302428217,8.07519857973553,0.501468424247686));
#7926=CARTESIAN_POINT('Ctrl Pts',(0.75598809315358,7.98909795455781,0.734610492596574));
#7927=CARTESIAN_POINT('Ctrl Pts',(0.798144520753771,7.74735667171032,1.38919415644391));
#7928=CARTESIAN_POINT('Ctrl Pts',(0.840300948353963,7.15085275059643,1.91274182910972));
#7929=CARTESIAN_POINT('Ctrl Pts',(0.882457375954154,6.47045143373377,2.06755669436143));
#7930=CARTESIAN_POINT('Ctrl Pts',(0.924613803554345,5.7900501168711,2.22237155961314));
#7931=CARTESIAN_POINT('Ctrl Pts',(0.966770231154535,5.02575140425966,2.00845361745078));
#7932=CARTESIAN_POINT('Ctrl Pts',(1.00892665875473,4.52458564392446,1.52292117702337));
#7933=CARTESIAN_POINT('Ctrl Pts',(1.05108308635492,4.02341988358925,1.03738873659595));
#7934=CARTESIAN_POINT('Ctrl Pts',(1.09323951395511,3.78538707553028,0.28024179790349));
#7935=CARTESIAN_POINT('Ctrl Pts',(1.1353959415553,3.91857305628055,-0.4047212890459));
#7936=CARTESIAN_POINT('Ctrl Pts',(1.17755236915549,4.05175903703082,-1.08968437599529));
#7937=CARTESIAN_POINT('Ctrl Pts',(1.21970879675568,4.55616380659031,-1.7024636112016));
#7938=CARTESIAN_POINT('Ctrl Pts',(1.26186522435587,5.20275434201912,-1.96482326042851));
#7939=CARTESIAN_POINT('Ctrl Pts',(1.30402165195606,5.84934487744794,-2.22718290965541));
#7940=CARTESIAN_POINT('Ctrl Pts',(1.34617807955625,6.63812117874606,-2.1391229729029));
#7941=CARTESIAN_POINT('Ctrl Pts',(1.38833450715645,7.21093149365039,-1.74062613827673));
#7942=CARTESIAN_POINT('Ctrl Pts',(1.4292042450968,7.76625861201282,-1.35429214063134));
#7943=CARTESIAN_POINT('Ctrl Pts',(1.47007398303714,8.11860189172077,-0.676182228442241));
#7944=CARTESIAN_POINT('Ctrl Pts',(1.51094372097749,8.12031955932164,0.000387557394038608));
#7945=CARTESIAN_POINT('Ctrl Pts',(0.,6.66173726856851,-2.47299490241842));
#7946=CARTESIAN_POINT('Ctrl Pts',(-2.92724575880526E-17,6.74302007470053,
-2.4435642830524));
#7947=CARTESIAN_POINT('Ctrl Pts',(-8.31564143722506E-17,6.82243058251537,
-2.40977680229731));
#7948=CARTESIAN_POINT('Ctrl Pts',(-7.97972798949331E-17,6.89976867880956,
-2.37194498173918));
#7949=CARTESIAN_POINT('Ctrl Pts',(-7.62437812158347E-17,6.98158166512527,
-2.33192415932525));
#7950=CARTESIAN_POINT('Ctrl Pts',(1.83719249610399E-16,7.06107643989013,
-2.2873769918661));
#7951=CARTESIAN_POINT('Ctrl Pts',(2.32452945780892E-16,7.13798362917082,
-2.23862239524585));
#7952=CARTESIAN_POINT('Ctrl Pts',(2.75094929930074E-16,7.20527741979142,
-2.19596212320313));
#7953=CARTESIAN_POINT('Ctrl Pts',(-3.13354561198216E-16,7.27058988911543,
-2.15007935982338));
#7954=CARTESIAN_POINT('Ctrl Pts',(-3.40005801291454E-16,7.33371319645899,
-2.10116340617892));
#7955=CARTESIAN_POINT('Ctrl Pts',(-3.52840359175394E-16,7.36411177225105,
-2.07760672978032));
#7956=CARTESIAN_POINT('Ctrl Pts',(1.0360295682957E-16,7.39400223353409,
-2.05334632697955));
#7957=CARTESIAN_POINT('Ctrl Pts',(1.31838984174237E-16,7.42335885067487,
-2.02840199034912));
#7958=CARTESIAN_POINT('Ctrl Pts',(1.49593456598285E-16,7.44181793640698,
-2.01271729322671));
#7959=CARTESIAN_POINT('Ctrl Pts',(-5.01310080724556E-17,7.46006591992173,
-1.99676217065983));
#7960=CARTESIAN_POINT('Ctrl Pts',(-5.55111512312578E-17,7.47809603849993,
-1.98054141094945));
#7961=CARTESIAN_POINT('Ctrl Pts',(-5.89928980535388E-17,7.48976418676514,
-1.97004418496315));
#7962=CARTESIAN_POINT('Ctrl Pts',(-3.27549090266268E-17,7.50134210697178,
-1.9594346195351));
#7963=CARTESIAN_POINT('Ctrl Pts',(-4.16333634234434E-17,7.51281285098918,
-1.94872845073444));
#7964=CARTESIAN_POINT('Ctrl Pts',(-9.07143297655421E-17,7.57622424849985,
-1.88954369998029));
#7965=CARTESIAN_POINT('Ctrl Pts',(-1.47034643718728E-16,7.63647286263829,
-1.82731287118978));
#7966=CARTESIAN_POINT('Ctrl Pts',(-1.2490009027033E-16,7.69332727300807,
-1.76231279717448));
#7967=CARTESIAN_POINT('Ctrl Pts',(-1.02897662229704E-16,7.74984230846473,
-1.69770072110568));
#7968=CARTESIAN_POINT('Ctrl Pts',(-4.18758661845513E-16,7.80300405366629,
-1.63035153777999));
#7969=CARTESIAN_POINT('Ctrl Pts',(-4.85722573273506E-16,7.85254163516931,
-1.56051042864998));
#7970=CARTESIAN_POINT('Ctrl Pts',(-5.45725005239589E-16,7.89692935536835,
-1.49792990864085));
#7971=CARTESIAN_POINT('Ctrl Pts',(1.03285777158662E-17,7.93840696580168,
-1.43334792061814));
#7972=CARTESIAN_POINT('Ctrl Pts',(-6.93889390390723E-17,7.97674451927385,
-1.3669303939457));
#7973=CARTESIAN_POINT('Ctrl Pts',(-1.05037396214999E-16,7.99388848823845,
-1.33722948940558));
#7974=CARTESIAN_POINT('Ctrl Pts',(1.79461103361955E-17,8.01040405398028,
-1.30716143593201));
#7975=CARTESIAN_POINT('Ctrl Pts',(5.55111512312578E-17,8.02626824247406,
-1.27674080217197));
#7976=CARTESIAN_POINT('Ctrl Pts',(7.37723601010594E-17,8.03398018029529,
-1.26195264984184));
#7977=CARTESIAN_POINT('Ctrl Pts',(-5.37222981174814E-16,8.04153816448487,
-1.24708117637209));
#7978=CARTESIAN_POINT('Ctrl Pts',(-5.55111512312578E-16,8.04893941986435,
-1.23212805327155));
#7979=CARTESIAN_POINT('Ctrl Pts',(-5.69642358968991E-16,8.05495145663562,
-1.21998163738446));
#7980=CARTESIAN_POINT('Ctrl Pts',(2.79116992920913E-16,8.06086026851682,
-1.20778075528828));
#7981=CARTESIAN_POINT('Ctrl Pts',(2.63677968348475E-16,8.06665780144445,
-1.19554063643636));
#7982=CARTESIAN_POINT('Ctrl Pts',(1.6930174401095E-16,8.10209716910752,
-1.12071879796678));
#7983=CARTESIAN_POINT('Ctrl Pts',(-3.46947901332591E-16,8.13344607811337,
-1.04430567332096));
#7984=CARTESIAN_POINT('Ctrl Pts',(-3.05311331771918E-16,8.16046085298837,
-0.96652813442685));
#7985=CARTESIAN_POINT('Ctrl Pts',(-2.63674762211246E-16,8.18747562786337,
-0.888750595532739));
#7986=CARTESIAN_POINT('Ctrl Pts',(-8.32710016965256E-17,8.21015673786416,
-0.809607920476006));
#7987=CARTESIAN_POINT('Ctrl Pts',(-2.77555756156289E-17,8.22820692560612,
-0.729317175418125));
#7988=CARTESIAN_POINT('Ctrl Pts',(2.8467517448409E-17,8.2464872029431,-0.648002947099096));
#7989=CARTESIAN_POINT('Ctrl Pts',(-1.24010162979355E-16,8.26001706827931,
-0.565509980237511));
#7990=CARTESIAN_POINT('Ctrl Pts',(-1.94289029309402E-16,8.26887071011419,
-0.48222934860738));
#7991=CARTESIAN_POINT('Ctrl Pts',(-2.1762897265876E-16,8.27181104637248,
-0.454571457610426));
#7992=CARTESIAN_POINT('Ctrl Pts',(-3.6803890847137E-16,8.27423521289526,
-0.426826800529392));
#7993=CARTESIAN_POINT('Ctrl Pts',(-3.88578058618805E-16,8.27614473190817,
-0.399010127625446));
#7994=CARTESIAN_POINT('Ctrl Pts',(-3.9982746972E-16,8.27719058649453,-0.383774775299874));
#7995=CARTESIAN_POINT('Ctrl Pts',(-7.62784563143259E-17,8.27808204622248,
-0.368517824314681));
#7996=CARTESIAN_POINT('Ctrl Pts',(-8.32667268468867E-17,8.27881928950886,
-0.353241737063793));
#7997=CARTESIAN_POINT('Ctrl Pts',(-8.92262223760452E-17,8.27944799986697,
-0.340214511908367));
#7998=CARTESIAN_POINT('Ctrl Pts',(1.13306245230702E-17,8.27996424640881,
-0.327178880475876));
#7999=CARTESIAN_POINT('Ctrl Pts',(2.77555756156289E-17,8.28036828922386,
-0.314144138808217));
#8000=CARTESIAN_POINT('Ctrl Pts',(1.30673503817005E-16,8.28290000144603,
-0.232469094571197));
#8001=CARTESIAN_POINT('Ctrl Pts',(8.32667268468867E-17,8.28103543097395,
-0.150734510285442));
#8002=CARTESIAN_POINT('Ctrl Pts',(8.32667268468867E-17,8.27490228926521,
-0.0693021198429901));
#8003=CARTESIAN_POINT('Ctrl Pts',(8.32667268468867E-17,8.26876142391814,
0.0122328207055393));
#8004=CARTESIAN_POINT('Ctrl Pts',(1.8500451461589E-16,8.25834084135165,
0.0934658284870283));
#8005=CARTESIAN_POINT('Ctrl Pts',(5.55111512312578E-17,8.24371805826975,
0.17402142364346));
#8006=CARTESIAN_POINT('Ctrl Pts',(-7.19074938173633E-17,8.22932955867074,
0.253286372190899));
#8007=CARTESIAN_POINT('Ctrl Pts',(6.41784410555287E-17,8.21087195899808,
0.331896311753077));
#8008=CARTESIAN_POINT('Ctrl Pts',(1.94289029309402E-16,8.18837667526648,
0.409467604336036));
#8009=CARTESIAN_POINT('Ctrl Pts',(2.4652271985269E-16,8.17934580618128,
0.440609073652239));
#8010=CARTESIAN_POINT('Ctrl Pts',(1.7445856536241E-16,8.16966375078697,
0.471582780693396));
#8011=CARTESIAN_POINT('Ctrl Pts',(1.66533453693773E-16,8.15933082804816,
0.502362225180225));
#8012=CARTESIAN_POINT('Ctrl Pts',(1.62901681143594E-16,8.15459564869234,
0.516467255654357));
#8013=CARTESIAN_POINT('Ctrl Pts',(6.62171881083989E-16,8.14972350969714,
0.530531944514346));
#8014=CARTESIAN_POINT('Ctrl Pts',(6.66133814775094E-16,8.14471983929536,
0.544539167387205));
#8015=CARTESIAN_POINT('Ctrl Pts',(6.87161873422234E-16,8.11816273792442,
0.618882840708986));
#8016=CARTESIAN_POINT('Ctrl Pts',(-1.24134177748354E-16,8.08787072716445,
0.691710604375033));
#8017=CARTESIAN_POINT('Ctrl Pts',(-2.77555756156289E-17,8.05389882723943,
0.762666289558938));
#8018=CARTESIAN_POINT('Ctrl Pts',(4.37166554604183E-17,8.02870602066407,
0.815285449988755));
#8019=CARTESIAN_POINT('Ctrl Pts',(5.91214766369708E-16,8.00148860185591,
0.866874658240732));
#8020=CARTESIAN_POINT('Ctrl Pts',(4.9960036108132E-16,7.97225570207189,
0.917275970722266));
#8021=CARTESIAN_POINT('Ctrl Pts',(4.67062548093405E-16,7.96187333236407,
0.935176523312302));
#8022=CARTESIAN_POINT('Ctrl Pts',(5.93084551578718E-16,7.95123663480896,
0.952927120175963));
#8023=CARTESIAN_POINT('Ctrl Pts',(6.10622663543836E-16,7.9403457074372,
0.970520278191213));
#8024=CARTESIAN_POINT('Ctrl Pts',(6.2283322446657E-16,7.93276311630981,
0.982769163829288));
#8025=CARTESIAN_POINT('Ctrl Pts',(5.89454364215472E-16,7.92505825553759,
0.994940049303588));
#8026=CARTESIAN_POINT('Ctrl Pts',(5.82867087928207E-16,7.91723622740492,
1.00702299437693));
#8027=CARTESIAN_POINT('Ctrl Pts',(5.48320440966256E-16,7.87621398503319,
1.07039140637391));
#8028=CARTESIAN_POINT('Ctrl Pts',(6.74760874961288E-16,7.83193489245364,
1.13140409419983));
#8029=CARTESIAN_POINT('Ctrl Pts',(5.55111512312578E-16,7.78442983090767,
1.18972080081364));
#8030=CARTESIAN_POINT('Ctrl Pts',(4.53551463141926E-16,7.74410687155662,
1.23922083541523));
#8031=CARTESIAN_POINT('Ctrl Pts',(2.26389524579989E-16,7.70145896228683,
1.28677814743062));
#8032=CARTESIAN_POINT('Ctrl Pts',(4.9960036108132E-16,7.65648804272845,
1.3321604106817));
#8033=CARTESIAN_POINT('Ctrl Pts',(5.66398646151588E-16,7.64543507438408,
1.34331447922279));
#8034=CARTESIAN_POINT('Ctrl Pts',(7.18591525774023E-17,7.63424170833627,
1.35433703657155));
#8035=CARTESIAN_POINT('Ctrl Pts',(5.55111512312578E-17,7.62291087731919,
1.3652268607858));
#8036=CARTESIAN_POINT('Origin',(6.,6.,0.));
#8037=CARTESIAN_POINT('Origin',(11.,-6.,0.));
#8038=CARTESIAN_POINT('Ctrl Pts',(11.,-4.63708777074269,-1.61992569438875));
#8039=CARTESIAN_POINT('Ctrl Pts',(11.,-4.68916071039273,-1.67389115040286));
#8040=CARTESIAN_POINT('Ctrl Pts',(11.,-4.74418227950824,-1.7247197028367));
#8041=CARTESIAN_POINT('Ctrl Pts',(11.,-4.80179350695765,-1.77240163479619));
#8042=CARTESIAN_POINT('Ctrl Pts',(11.,-4.86093069393025,-1.8213465271434));
#8043=CARTESIAN_POINT('Ctrl Pts',(11.,-4.92279707407985,-1.86697639170717));
#8044=CARTESIAN_POINT('Ctrl Pts',(11.,-4.98704961307706,-1.9092500417527));
#8045=CARTESIAN_POINT('Ctrl Pts',(11.,-5.0009412869431,-1.91838978578032));
#8046=CARTESIAN_POINT('Ctrl Pts',(11.,-5.01494649271969,-1.92737366922165));
#8047=CARTESIAN_POINT('Ctrl Pts',(11.,-5.02905605736331,-1.93619735983612));
#8048=CARTESIAN_POINT('Ctrl Pts',(11.,-5.095826994682,-1.97795386386861));
#8049=CARTESIAN_POINT('Ctrl Pts',(11.,-5.16480894835441,-2.01605026992946));
#8050=CARTESIAN_POINT('Ctrl Pts',(11.,-5.23562552815997,-2.05045819483435));
#8051=CARTESIAN_POINT('Ctrl Pts',(11.,-5.29121456335243,-2.07746745387636));
#8052=CARTESIAN_POINT('Ctrl Pts',(11.,-5.34793515199878,-2.10220338751318));
#8053=CARTESIAN_POINT('Ctrl Pts',(11.,-5.40562122838672,-2.12463650733759));
#8054=CARTESIAN_POINT('Ctrl Pts',(11.,-5.42503819593862,-2.13218743100917));
#8055=CARTESIAN_POINT('Ctrl Pts',(11.,-5.44456464967012,-2.13947732652672));
#8056=CARTESIAN_POINT('Ctrl Pts',(11.,-5.46419453130331,-2.14650467737314));
#8057=CARTESIAN_POINT('Ctrl Pts',(11.,-5.48077911786492,-2.15244183535448));
#8058=CARTESIAN_POINT('Ctrl Pts',(11.,-5.49743964788631,-2.15819215670317));
#8059=CARTESIAN_POINT('Ctrl Pts',(11.,-5.5141504139477,-2.16374765702697));
#8060=CARTESIAN_POINT('Ctrl Pts',(11.,-5.59091180623393,-2.18926701012754));
#8061=CARTESIAN_POINT('Ctrl Pts',(11.,-5.66882884756264,-2.21071518477414));
#8062=CARTESIAN_POINT('Ctrl Pts',(11.,-5.74752223865727,-2.22806242052001));
#8063=CARTESIAN_POINT('Ctrl Pts',(11.,-5.82735436949371,-2.24566068098954));
#8064=CARTESIAN_POINT('Ctrl Pts',(11.,-5.90798634098841,-2.25903895400364));
#8065=CARTESIAN_POINT('Ctrl Pts',(11.,-5.98905364152142,-2.26812340437189));
#8066=CARTESIAN_POINT('Ctrl Pts',(11.,-6.06934098436991,-2.27712045221375));
#8067=CARTESIAN_POINT('Ctrl Pts',(11.,-6.15005628953376,-2.28190623150704));
#8068=CARTESIAN_POINT('Ctrl Pts',(11.,-6.2308622507703,-2.28236146501133));
#8069=CARTESIAN_POINT('Ctrl Pts',(11.,-6.26376631466807,-2.28254683539842));
#8070=CARTESIAN_POINT('Ctrl Pts',(11.,-6.29668552386031,-2.28201357588125));
#8071=CARTESIAN_POINT('Ctrl Pts',(11.,-6.32959734487964,-2.28075114470524));
#8072=CARTESIAN_POINT('Ctrl Pts',(11.,-6.34313630322685,-2.28023181752799));
#8073=CARTESIAN_POINT('Ctrl Pts',(11.,-6.3566759153337,-2.27958889854899));
#8074=CARTESIAN_POINT('Ctrl Pts',(11.,-6.37019720730564,-2.27882277952366));
#8075=CARTESIAN_POINT('Ctrl Pts',(11.,-6.45384130154684,-2.27408348892273));
#8076=CARTESIAN_POINT('Ctrl Pts',(11.,-6.53692139016417,-2.2646296568094));
#8077=CARTESIAN_POINT('Ctrl Pts',(11.,-6.61905941956099,-2.25039732976414));
#8078=CARTESIAN_POINT('Ctrl Pts',(11.,-6.63843261915327,-2.24704047162504));
#8079=CARTESIAN_POINT('Ctrl Pts',(11.,-6.65775349179807,-2.24341756918389));
#8080=CARTESIAN_POINT('Ctrl Pts',(11.,-6.67701720133506,-2.2395273783889));
#8081=CARTESIAN_POINT('Ctrl Pts',(11.,-6.75568871853955,-2.22364013655372));
#8082=CARTESIAN_POINT('Ctrl Pts',(11.,-6.83340685342578,-2.20329917928858));
#8083=CARTESIAN_POINT('Ctrl Pts',(11.,-6.90995038418047,-2.17879339655753));
#8084=CARTESIAN_POINT('Ctrl Pts',(11.,-6.98825812324156,-2.15372279397793));
#8085=CARTESIAN_POINT('Ctrl Pts',(11.,-7.06533723375411,-2.12429291956538));
#8086=CARTESIAN_POINT('Ctrl Pts',(11.,-7.14094474113465,-2.09075923730983));
#8087=CARTESIAN_POINT('Ctrl Pts',(11.,-7.15790725065089,-2.0832359711147));
#8088=CARTESIAN_POINT('Ctrl Pts',(11.,-7.17479564031027,-2.07550594796968));
#8089=CARTESIAN_POINT('Ctrl Pts',(11.,-7.19160706411186,-2.06757171297803));
#8090=CARTESIAN_POINT('Ctrl Pts',(11.,-7.20870424201776,-2.05950261491706));
#8091=CARTESIAN_POINT('Ctrl Pts',(11.,-7.2257270756284,-2.05121953031441));
#8092=CARTESIAN_POINT('Ctrl Pts',(11.,-7.24264281162302,-2.04274031453622));
#8093=CARTESIAN_POINT('Ctrl Pts',(11.,-7.31794347071332,-2.00499495501592));
#8094=CARTESIAN_POINT('Ctrl Pts',(11.,-7.39121475588854,-1.96332675494362));
#8095=CARTESIAN_POINT('Ctrl Pts',(11.,-7.46222053368768,-1.91806519793764));
#8096=CARTESIAN_POINT('Ctrl Pts',(11.,-7.53467721725653,-1.8718787830364));
#8097=CARTESIAN_POINT('Ctrl Pts',(11.,-7.60477566895564,-1.82195030921268));
#8098=CARTESIAN_POINT('Ctrl Pts',(11.,-7.67225632822043,-1.76857519958011));
#8099=CARTESIAN_POINT('Ctrl Pts',(11.,-7.7402204116953,-1.71481771638312));
#8100=CARTESIAN_POINT('Ctrl Pts',(11.,-7.80552992851377,-1.65756352815942));
#8101=CARTESIAN_POINT('Ctrl Pts',(11.,-7.86789832115903,-1.597066268732));
#8102=CARTESIAN_POINT('Ctrl Pts',(11.,-7.88758899419526,-1.57796634159826));
#8103=CARTESIAN_POINT('Ctrl Pts',(11.,-7.90698629455484,-1.55854283015653));
#8104=CARTESIAN_POINT('Ctrl Pts',(11.,-7.92608054802242,-1.53880285675951));
#8105=CARTESIAN_POINT('Ctrl Pts',(11.,-7.93886127755718,-1.52558991489516));
#8106=CARTESIAN_POINT('Ctrl Pts',(11.,-7.95150622626967,-1.51223518086157));
#8107=CARTESIAN_POINT('Ctrl Pts',(11.,-7.96401239792668,-1.49874069798903));
#8108=CARTESIAN_POINT('Ctrl Pts',(11.,-7.97296243208598,-1.48908337950791));
#8109=CARTESIAN_POINT('Ctrl Pts',(11.,-7.98184040084489,-1.47935546066086));
#8110=CARTESIAN_POINT('Ctrl Pts',(11.,-7.99063713711847,-1.46956699588278));
#8111=CARTESIAN_POINT('Ctrl Pts',(11.,-8.05020603751975,-1.40328240290278));
#8112=CARTESIAN_POINT('Ctrl Pts',(11.,-8.10615530524682,-1.33411428433584));
#8113=CARTESIAN_POINT('Ctrl Pts',(11.,-8.15821728462088,-1.26237772980875));
#8114=CARTESIAN_POINT('Ctrl Pts',(11.,-8.21030973545835,-1.19059918844553));
#8115=CARTESIAN_POINT('Ctrl Pts',(11.,-8.25851120867521,-1.11624858408148));
#8116=CARTESIAN_POINT('Ctrl Pts',(11.,-8.30252641897689,-1.03959725091855));
#8117=CARTESIAN_POINT('Ctrl Pts',(11.,-8.34556791606098,-0.964641613760129));
#8118=CARTESIAN_POINT('Ctrl Pts',(11.,-8.38460699954129,-0.88748521250845));
#8119=CARTESIAN_POINT('Ctrl Pts',(11.,-8.41933041215152,-0.808349409023425));
#8120=CARTESIAN_POINT('Ctrl Pts',(11.,-8.43267483371714,-0.777937031804278));
#8121=CARTESIAN_POINT('Ctrl Pts',(11.,-8.4453814194259,-0.74723202383003));
#8122=CARTESIAN_POINT('Ctrl Pts',(11.,-8.45743055670488,-0.716245966456263));
#8123=CARTESIAN_POINT('Ctrl Pts',(11.,-8.46428526209977,-0.69861812392042));
#8124=CARTESIAN_POINT('Ctrl Pts',(11.,-8.47092716798352,-0.680899312562034));
#8125=CARTESIAN_POINT('Ctrl Pts',(11.,-8.47735703821271,-0.663092892961399));
#8126=CARTESIAN_POINT('Ctrl Pts',(11.,-8.47299490241841,0.661737268568549));
#8127=CARTESIAN_POINT('Ctrl Pts',(11.,-8.44299217193241,0.744600156882087));
#8128=CARTESIAN_POINT('Ctrl Pts',(11.,-8.40842658662345,0.825613049231886));
#8129=CARTESIAN_POINT('Ctrl Pts',(11.,-8.36960246891694,0.904544308645214));
#8130=CARTESIAN_POINT('Ctrl Pts',(11.,-8.32947621078867,0.986122880850064));
#8131=CARTESIAN_POINT('Ctrl Pts',(11.,-8.28480032785149,1.06547870562738));
#8132=CARTESIAN_POINT('Ctrl Pts',(11.,-8.23586758286413,1.14231964012019));
#8133=CARTESIAN_POINT('Ctrl Pts',(11.,-8.22619772360642,1.15750458472054));
#8134=CARTESIAN_POINT('Ctrl Pts',(11.,-8.21636151332297,1.17259118394073));
#8135=CARTESIAN_POINT('Ctrl Pts',(11.,-8.20636105572507,1.18757697609823));
#8136=CARTESIAN_POINT('Ctrl Pts',(11.,-8.19636269232515,1.20255963007776));
#8137=CARTESIAN_POINT('Ctrl Pts',(11.,-8.18620566899149,1.21743322439163));
#8138=CARTESIAN_POINT('Ctrl Pts',(11.,-8.17589375376841,1.23219396468862));
#8139=CARTESIAN_POINT('Ctrl Pts',(11.,-8.12540468254945,1.30446531797046));
#8140=CARTESIAN_POINT('Ctrl Pts',(11.,-8.07119588129312,1.37404838032795));
#8141=CARTESIAN_POINT('Ctrl Pts',(11.,-8.0135480096579,1.44068419309266));
#8142=CARTESIAN_POINT('Ctrl Pts',(11.,-7.97155389150282,1.48922565898246));
#8143=CARTESIAN_POINT('Ctrl Pts',(11.,-7.92773394870726,1.53620245880582));
#8144=CARTESIAN_POINT('Ctrl Pts',(11.,-7.88218714794513,1.58149989349267));
#8145=CARTESIAN_POINT('Ctrl Pts',(11.,-7.86583399269375,1.5977635161737));
#8146=CARTESIAN_POINT('Ctrl Pts',(11.,-7.84925816751652,1.61381052543022));
#8147=CARTESIAN_POINT('Ctrl Pts',(11.,-7.83246407288259,1.62963517198371));
#8148=CARTESIAN_POINT('Ctrl Pts',(11.,-7.82132717922489,1.64012918250814));
#8149=CARTESIAN_POINT('Ctrl Pts',(11.,-7.81010043989387,1.65051957759726));
#8150=CARTESIAN_POINT('Ctrl Pts',(11.,-7.79878879465207,1.66080200414467));
#8151=CARTESIAN_POINT('Ctrl Pts',(11.,-7.73504595251212,1.71874504233381));
#8152=CARTESIAN_POINT('Ctrl Pts',(11.,-7.66857522386929,1.77329518611919));
#8153=CARTESIAN_POINT('Ctrl Pts',(11.,-7.59964161110829,1.82421541577063));
#8154=CARTESIAN_POINT('Ctrl Pts',(11.,-7.53207142409031,1.87412850319976));
#8155=CARTESIAN_POINT('Ctrl Pts',(11.,-7.46213399626932,1.92055421440432));
#8156=CARTESIAN_POINT('Ctrl Pts',(11.,-7.39005745111888,1.96322512488115));
#8157=CARTESIAN_POINT('Ctrl Pts',(11.,-7.31945832744952,2.00502136913163));
#8158=CARTESIAN_POINT('Ctrl Pts',(11.,-7.2468061944969,2.04321546128308));
#8159=CARTESIAN_POINT('Ctrl Pts',(11.,-7.17230561691982,2.07750845132568));
#8160=CARTESIAN_POINT('Ctrl Pts',(11.,-7.15028246724394,2.08764581773415));
#8161=CARTESIAN_POINT('Ctrl Pts',(11.,-7.12809776072295,2.09744194614622));
#8162=CARTESIAN_POINT('Ctrl Pts',(11.,-7.10575674483513,2.10688823607142));
#8163=CARTESIAN_POINT('Ctrl Pts',(11.,-7.08863683070083,2.11412692536018));
#8164=CARTESIAN_POINT('Ctrl Pts',(11.,-7.0714251291155,2.12116017596557));
#8165=CARTESIAN_POINT('Ctrl Pts',(11.,-7.05412400850806,2.12798394870633));
#8166=CARTESIAN_POINT('Ctrl Pts',(11.,-7.0421560960086,2.1327042391968));
#8167=CARTESIAN_POINT('Ctrl Pts',(11.,-7.0301482296559,2.13732310976275));
#8168=CARTESIAN_POINT('Ctrl Pts',(11.,-7.01811087072427,2.14183590822721));
#8169=CARTESIAN_POINT('Ctrl Pts',(11.,-6.94192107660596,2.17039941521055));
#8170=CARTESIAN_POINT('Ctrl Pts',(11.,-6.86443967890492,2.19476166022804));
#8171=CARTESIAN_POINT('Ctrl Pts',(11.,-6.78588043231568,2.21467983405259));
#8172=CARTESIAN_POINT('Ctrl Pts',(11.,-6.76708719688578,2.2194447337464));
#8173=CARTESIAN_POINT('Ctrl Pts',(11.,-6.74823223066446,2.22395507969414));
#8174=CARTESIAN_POINT('Ctrl Pts',(11.,-6.72931838764412,2.22820710552603));
#8175=CARTESIAN_POINT('Ctrl Pts',(11.,-6.64883815143219,2.24629988777883));
#8176=CARTESIAN_POINT('Ctrl Pts',(11.,-6.56729156100039,2.25971968137586));
#8177=CARTESIAN_POINT('Ctrl Pts',(11.,-6.48505615285959,2.26856864579746));
#8178=CARTESIAN_POINT('Ctrl Pts',(11.,-6.40338815460454,2.27735655391734));
#8179=CARTESIAN_POINT('Ctrl Pts',(11.,-6.32103982649442,2.28163608098665));
#8180=CARTESIAN_POINT('Ctrl Pts',(11.,-6.23839365107816,2.28145912099538));
#8181=CARTESIAN_POINT('Ctrl Pts',(11.,-6.21813581056131,2.28141574539739));
#8182=CARTESIAN_POINT('Ctrl Pts',(11.,-6.19786017422479,2.28110440549847));
#8183=CARTESIAN_POINT('Ctrl Pts',(11.,-6.17757259598781,2.28052546242847));
#8184=CARTESIAN_POINT('Ctrl Pts',(11.,-6.16489228263999,2.28016360654541));
#8185=CARTESIAN_POINT('Ctrl Pts',(11.,-6.15220804476619,2.27969715540688));
#8186=CARTESIAN_POINT('Ctrl Pts',(11.,-6.13953434549051,2.27912700305166));
#8187=CARTESIAN_POINT('Ctrl Pts',(11.,-6.05806362624421,2.27546187565287));
#8188=CARTESIAN_POINT('Ctrl Pts',(11.,-5.976885766891,2.26751233932642));
#8189=CARTESIAN_POINT('Ctrl Pts',(11.,-5.89635941922123,2.25539762204348));
#8190=CARTESIAN_POINT('Ctrl Pts',(11.,-5.81599843329012,2.24330778246543));
#8191=CARTESIAN_POINT('Ctrl Pts',(11.,-5.73628529198131,2.22706943595767));
#8192=CARTESIAN_POINT('Ctrl Pts',(11.,-5.65759278366309,2.20675219816744));
#8193=CARTESIAN_POINT('Ctrl Pts',(11.,-5.58032860266213,2.18680373329304));
#8194=CARTESIAN_POINT('Ctrl Pts',(11.,-5.50404751923812,2.16292262378908));
#8195=CARTESIAN_POINT('Ctrl Pts',(11.,-5.42913146009419,2.13513438322616));
#8196=CARTESIAN_POINT('Ctrl Pts',(11.,-5.39726310244459,2.12331361210136));
#8197=CARTESIAN_POINT('Ctrl Pts',(11.,-5.36564218650334,2.11078536423984));
#8198=CARTESIAN_POINT('Ctrl Pts',(11.,-5.3343002956742,2.09754964276009));
#8199=CARTESIAN_POINT('Ctrl Pts',(11.,-5.32160465228749,2.09218825595708));
#8200=CARTESIAN_POINT('Ctrl Pts',(11.,-5.30895358614716,2.08671013786179));
#8201=CARTESIAN_POINT('Ctrl Pts',(11.,-5.2963657193717,2.08112281913911));
#8202=CARTESIAN_POINT('Ctrl Pts',(11.,-5.22470595288081,2.0493155270761));
#8203=CARTESIAN_POINT('Ctrl Pts',(11.,-5.1549687226797,2.0139219178475));
#8204=CARTESIAN_POINT('Ctrl Pts',(11.,-5.08749005705245,1.97501188775492));
#8205=CARTESIAN_POINT('Ctrl Pts',(11.,-5.02118530622618,1.93677876879874));
#8206=CARTESIAN_POINT('Ctrl Pts',(11.,-4.95706050256354,1.8951500455755));
#8207=CARTESIAN_POINT('Ctrl Pts',(11.,-4.89546768821356,1.85015506607012));
#8208=CARTESIAN_POINT('Ctrl Pts',(11.,-4.8358598511882,1.80661015854118));
#8209=CARTESIAN_POINT('Ctrl Pts',(11.,-4.77862296475962,1.75991201329989));
#8210=CARTESIAN_POINT('Ctrl Pts',(11.,-4.72411594487011,1.7100591248934));
#8211=CARTESIAN_POINT('Ctrl Pts',(11.,-4.70501584604852,1.6925899053867));
#8212=CARTESIAN_POINT('Ctrl Pts',(11.,-4.68625134890234,1.67473308433625));
#8213=CARTESIAN_POINT('Ctrl Pts',(11.,-4.66783926694922,1.65648789471542));
#8214=CARTESIAN_POINT('Ctrl Pts',(11.,-4.6566873428301,1.64543705479909));
#8215=CARTESIAN_POINT('Ctrl Pts',(11.,-4.64566472044625,1.63424373084128));
#8216=CARTESIAN_POINT('Ctrl Pts',(11.,-4.63477280471478,1.62291072646336));
#8217=CARTESIAN_POINT('Origin',(-1.7667098902285,-6.,0.));
#8218=CARTESIAN_POINT('Ctrl Pts',(0.233290109771496,-3.4375580541705,0.00169662369046201));
#8219=CARTESIAN_POINT('Ctrl Pts',(0.238897060498093,-3.43666696742173,0.114092740073729));
#8220=CARTESIAN_POINT('Ctrl Pts',(0.286660438824881,-3.49427689386692,1.07067089040277));
#8221=CARTESIAN_POINT('Ctrl Pts',(0.376580244751861,-4.69833585942183,2.72694181908363));
#8222=CARTESIAN_POINT('Ctrl Pts',(0.503049527552434,-7.57381067700105,2.57901747640416));
#8223=CARTESIAN_POINT('Ctrl Pts',(0.629518810353007,-9.02010634361806,0.0895593516203334));
#8224=CARTESIAN_POINT('Ctrl Pts',(0.755988093153582,-7.72375616695671,-2.48150715181869));
#8225=CARTESIAN_POINT('Ctrl Pts',(0.882457375954152,-4.86203286070258,-2.79891511344676));
#8226=CARTESIAN_POINT('Ctrl Pts',(0.97489138149346,-3.52575264953356,-1.17323436387186));
#8227=CARTESIAN_POINT('Ctrl Pts',(1.02516895943257,-3.43750802030871,-0.165257814947204));
#8228=CARTESIAN_POINT('Ctrl Pts',(1.0332901097715,-3.438979209753,-0.00218674096624601));
#8229=CARTESIAN_POINT('Ctrl Pts',(0.166709890228505,-3.44261795854501,-0.00304121041534603));
#8230=CARTESIAN_POINT('Ctrl Pts',(0.195452782019385,-3.44686084504951,0.576034429433346));
#8231=CARTESIAN_POINT('Ctrl Pts',(0.266352101410457,-3.92613180196041,2.01289446940098));
#8232=CARTESIAN_POINT('Ctrl Pts',(0.379407848401719,-6.30137623450992,3.00550525361278));
#8233=CARTESIAN_POINT('Ctrl Pts',(0.505877131202293,-8.68279501755112,1.3897499208415));
#8234=CARTESIAN_POINT('Ctrl Pts',(0.632346414002865,-8.62891891149828,-1.48974040295355));
#8235=CARTESIAN_POINT('Ctrl Pts',(0.758815696803439,-6.18713281460021,-3.01549224619728));
#8236=CARTESIAN_POINT('Ctrl Pts',(0.870270188878651,-3.8857217769571,-1.94718070444853));
#8237=CARTESIAN_POINT('Ctrl Pts',(0.939568253353674,-3.44623974036578,-0.545331334169339));
#8238=CARTESIAN_POINT('Ctrl Pts',(0.966709890228505,-3.4427709916825,0.00173622513077922));
#8239=CARTESIAN_POINT('Ctrl Pts',(-2.77555756156289E-16,-7.61992569438872,
1.36291222925734));
#8240=CARTESIAN_POINT('Ctrl Pts',(0.0421564276001907,-8.07118022033932,
0.826561622369841));
#8241=CARTESIAN_POINT('Ctrl Pts',(0.126469282800573,-8.39177520902806,-0.720175462073977));
#8242=CARTESIAN_POINT('Ctrl Pts',(0.252938565601146,-6.69918148311235,-2.40042657120791));
#8243=CARTESIAN_POINT('Ctrl Pts',(0.379407848401718,-4.37212097158592,-1.89456935454149));
#8244=CARTESIAN_POINT('Ctrl Pts',(0.505877131202293,-3.52316464584869,0.328673032761782));
#8245=CARTESIAN_POINT('Ctrl Pts',(0.632346414002864,-4.92358477124844,2.25505305898439));
#8246=CARTESIAN_POINT('Ctrl Pts',(0.758815696803439,-7.30146765750439,2.13272656154203));
#8247=CARTESIAN_POINT('Ctrl Pts',(0.88528497960401,-8.49748637868727,0.074061385695407));
#8248=CARTESIAN_POINT('Ctrl Pts',(1.01175426240459,-7.42546554900288,-2.05209009390631));
#8249=CARTESIAN_POINT('Ctrl Pts',(1.13822354520516,-5.05895451801068,-2.31457159967453));
#8250=CARTESIAN_POINT('Ctrl Pts',(1.26469282800573,-3.54702442124209,-0.475200162100537));
#8251=CARTESIAN_POINT('Ctrl Pts',(1.3911621108063,-4.26269984665637,1.79574416585738));
#8252=CARTESIAN_POINT('Ctrl Pts',(1.51763139360688,-6.55605629257995,2.43591492214283));
#8253=CARTESIAN_POINT('Ctrl Pts',(1.64410067640745,-8.34444584030976,0.863984381349539));
#8254=CARTESIAN_POINT('Ctrl Pts',(1.77056995920802,-8.00379002929963,-1.49255486462238));
#8255=CARTESIAN_POINT('Ctrl Pts',(1.8970392420086,-5.84344667754611,-2.49366835649056));
#8256=CARTESIAN_POINT('Ctrl Pts',(2.02350852480917,-3.82527290719829,-1.23022567500147));
#8257=CARTESIAN_POINT('Ctrl Pts',(2.14997780760974,-3.78201874786567,1.15041383249752));
#8258=CARTESIAN_POINT('Ctrl Pts',(2.27644709041031,-5.75296422837819,2.48633579704923));
#8259=CARTESIAN_POINT('Ctrl Pts',(2.40291637321089,-7.9482485726293,1.56435936173015));
#8260=CARTESIAN_POINT('Ctrl Pts',(2.52938565601146,-8.37428368311575,-0.778247796073561));
#8261=CARTESIAN_POINT('Ctrl Pts',(2.65585493881204,-6.6441773108105,-2.41411022529385));
#8262=CARTESIAN_POINT('Ctrl Pts',(2.78232422161261,-4.3290787414722,-1.85766379771369));
#8263=CARTESIAN_POINT('Ctrl Pts',(2.90879350441318,-3.53138210395009,0.38576975861922));
#8264=CARTESIAN_POINT('Ctrl Pts',(3.03526278721376,-4.97549401505624,2.27887693933677));
#8265=CARTESIAN_POINT('Ctrl Pts',(3.16173207001432,-7.3499833166459,2.10248369069325));
#8266=CARTESIAN_POINT('Ctrl Pts',(3.2882013528149,-8.49852179549707,0.0167767631624936));
#8267=CARTESIAN_POINT('Ctrl Pts',(3.41467063561548,-7.37809530815189,-2.08416552689859));
#8268=CARTESIAN_POINT('Ctrl Pts',(3.54113991841604,-5.00618885369701,-2.29242928534551));
#8269=CARTESIAN_POINT('Ctrl Pts',(3.66760920121662,-3.53678510230054,-0.418885414119979));
#8270=CARTESIAN_POINT('Ctrl Pts',(3.79407848401719,-4.30428331321763,1.83505791204326));
#8271=CARTESIAN_POINT('Ctrl Pts',(3.92054776681776,-6.61170075236032,2.4225430464854));
#8272=CARTESIAN_POINT('Ctrl Pts',(4.04701704961834,-8.36361870398636,0.810061259790201));
#8273=CARTESIAN_POINT('Ctrl Pts',(4.1734863324189,-7.96908028184454,-1.53805574219553));
#8274=CARTESIAN_POINT('Ctrl Pts',(4.29995561521949,-5.78637487900414,-2.48942903697728));
#8275=CARTESIAN_POINT('Ctrl Pts',(4.42642489802005,-3.7976673497574,-1.18009470811942));
#8276=CARTESIAN_POINT('Ctrl Pts',(4.55289418082064,-3.80894862847708,1.20091070017914));
#8277=CARTESIAN_POINT('Ctrl Pts',(4.6793634636212,-5.80997392713084,2.49134154906332));
#8278=CARTESIAN_POINT('Ctrl Pts',(4.80583274642178,-7.98356626233935,1.51932797820845));
#8279=CARTESIAN_POINT('Ctrl Pts',(4.93230202922234,-8.35583656560968,-0.832422187711553));
#8280=CARTESIAN_POINT('Ctrl Pts',(5.05877131202293,-6.58871763351688,-2.42823066664694));
#8281=CARTESIAN_POINT('Ctrl Pts',(5.18524059482349,-4.28697071143509,-1.81890716612392));
#8282=CARTESIAN_POINT('Ctrl Pts',(5.31170987762408,-3.54086498845706,0.442207663278129));
#8283=CARTESIAN_POINT('Ctrl Pts',(5.43817916042463,-5.02795618957805,2.30174356805414));
#8284=CARTESIAN_POINT('Ctrl Pts',(5.56464844322522,-7.39778267661641,2.07101332960685));
#8285=CARTESIAN_POINT('Ctrl Pts',(5.69111772602579,-8.49825064558784,-0.0404516288687811));
#8286=CARTESIAN_POINT('Ctrl Pts',(5.81758700882636,-7.32999988575116,-2.11518153508395));
#8287=CARTESIAN_POINT('Ctrl Pts',(5.94405629162693,-4.95394571537787,-2.2690665605226));
#8288=CARTESIAN_POINT('Ctrl Pts',(6.07052557442751,-3.52783744057095,-0.362360182988378));
#8289=CARTESIAN_POINT('Ctrl Pts',(6.19699485722807,-4.34675670499038,1.87341379037416));
#8290=CARTESIAN_POINT('Ctrl Pts',(6.32346414002865,-6.66702413609162,2.40789771882639));
#8291=CARTESIAN_POINT('Ctrl Pts',(6.44993342282923,-8.38155164562368,0.7557144842366));
#8292=CARTESIAN_POINT('Ctrl Pts',(6.57640270562979,-7.93333746564924,-1.58275041190211));
#8293=CARTESIAN_POINT('Ctrl Pts',(6.70287198843038,-5.72941517641325,-2.48388334583205));
#8294=CARTESIAN_POINT('Ctrl Pts',(6.82934127123094,-3.77121717352535,-1.12934482549294));
#8295=CARTESIAN_POINT('Ctrl Pts',(6.95581055403152,-3.83702799048622,1.25077764151987));
#8296=CARTESIAN_POINT('Ctrl Pts',(7.08227983683208,-5.86708331451848,2.49504023558143));
#8297=CARTESIAN_POINT('Ctrl Pts',(7.20874911963267,-8.01784333014474,1.47349954782397));
#8298=CARTESIAN_POINT('Ctrl Pts',(7.33521840243323,-8.33615352215498,-0.886159885932465));
#8299=CARTESIAN_POINT('Ctrl Pts',(7.46168768523382,-6.53294910211921,-2.44107719602128));
#8300=CARTESIAN_POINT('Ctrl Pts',(7.58815696803438,-4.24576137502258,-1.7791962986271));
#8301=CARTESIAN_POINT('Ctrl Pts',(7.71462625083496,-3.55163799077159,0.49841357785763));
#8302=CARTESIAN_POINT('Ctrl Pts',(7.84109553363553,-5.08092832028779,2.32340264900719));
#8303=CARTESIAN_POINT('Ctrl Pts',(7.9675648164361,-7.44484872802906,2.03845646886778));
#8304=CARTESIAN_POINT('Ctrl Pts',(8.09403409923668,-8.4966688574394,-0.0976587996322113));
#8305=CARTESIAN_POINT('Ctrl Pts',(8.22050338203724,-7.28120671449707,-2.14508787059042));
#8306=CARTESIAN_POINT('Ctrl Pts',(8.34697266483783,-4.90225136246375,-2.24451343327464));
#8307=CARTESIAN_POINT('Ctrl Pts',(8.47344194763839,-3.5201867278485,-0.305644847490535));
#8308=CARTESIAN_POINT('Ctrl Pts',(8.59991123043897,-4.39009743180727,1.91078682970075));
#8309=CARTESIAN_POINT('Ctrl Pts',(8.72638051323955,-6.72199757186506,2.39198916097544));
#8310=CARTESIAN_POINT('Ctrl Pts',(8.85284979604012,-8.39823519454311,0.700971229823036));
#8311=CARTESIAN_POINT('Ctrl Pts',(8.97931907884069,-7.89658033286896,-1.62661470825881));
#8312=CARTESIAN_POINT('Ctrl Pts',(9.10578836164127,-5.67259751314697,-2.47703460460759));
#8313=CARTESIAN_POINT('Ctrl Pts',(9.23225764444182,-3.74593610549994,-1.07800236507619));
#8314=CARTESIAN_POINT('Ctrl Pts',(9.35872692724242,-3.86624240572105,1.29998820909676));
#8315=CARTESIAN_POINT('Ctrl Pts',(9.48519621004297,-5.92426184101915,2.49743032669638));
#8316=CARTESIAN_POINT('Ctrl Pts',(9.61166549284356,-8.05106292487872,1.42689739909694));
#8317=CARTESIAN_POINT('Ctrl Pts',(9.73813477564412,-8.31524271099646,-0.939431369294025));
#8318=CARTESIAN_POINT('Ctrl Pts',(9.8646040584447,-6.47690512487916,-2.45264559891613));
#8319=CARTESIAN_POINT('Ctrl Pts',(9.99107334124527,-4.20546440592863,-1.73854720547185));
#8320=CARTESIAN_POINT('Ctrl Pts',(10.1175426240458,-3.56371066804312,0.554348789288414));
#8321=CARTESIAN_POINT('Ctrl Pts',(10.2440119068464,-5.1343535056252,2.34386047615449));
#8322=CARTESIAN_POINT('Ctrl Pts',(10.370481189647,-7.49121250041255,2.0047963934507));
#8323=CARTESIAN_POINT('Ctrl Pts',(10.4969504724476,-8.49367060210842,-0.154750050135963));
#8324=CARTESIAN_POINT('Ctrl Pts',(10.6234197552481,-7.23194557971607,-2.17399267067328));
#8325=CARTESIAN_POINT('Ctrl Pts',(10.7498890380487,-4.85074177411285,-2.21854566422902));
#8326=CARTESIAN_POINT('Ctrl Pts',(10.8763583208493,-3.51458845010521,-0.249223991557292));
#8327=CARTESIAN_POINT('Ctrl Pts',(11.0028276036499,-4.43281921636254,1.94803666841403));
#8328=CARTESIAN_POINT('Ctrl Pts',(11.1292968864504,-6.77961885270218,2.37306464117732));
#8329=CARTESIAN_POINT('Ctrl Pts',(11.2136097416508,-7.86386672657618,1.22433347020397));
#8330=CARTESIAN_POINT('Ctrl Pts',(11.255766169251,-8.04505086266397,0.547225702171725));
#8331=CARTESIAN_POINT('Ctrl Pts',(-0.085255389750335,-7.73292003899811,
1.45797916636347));
#8332=CARTESIAN_POINT('Ctrl Pts',(-0.043098962150144,-8.21565082931591,
0.884216605633869));
#8333=CARTESIAN_POINT('Ctrl Pts',(0.0412138930502382,-8.55860821447594,
-0.770409713325555));
#8334=CARTESIAN_POINT('Ctrl Pts',(0.167683175850811,-6.74795134565662,-2.56786303334696));
#8335=CARTESIAN_POINT('Ctrl Pts',(0.294152458651384,-4.25857185970001,-2.02672086203038));
#8336=CARTESIAN_POINT('Ctrl Pts',(0.420621741451957,-3.35039845754936,0.351598895383963));
#8337=CARTESIAN_POINT('Ctrl Pts',(0.547091024252531,-4.84850180063956,2.4123493123508));
#8338=CARTESIAN_POINT('Ctrl Pts',(0.673560307053103,-7.39224866400329,2.28149019982941));
#8339=CARTESIAN_POINT('Ctrl Pts',(0.800029589853677,-8.67169303366418,0.079227374337048));
#8340=CARTESIAN_POINT('Ctrl Pts',(0.926498872654249,-7.52489575498751,-2.19522911321044));
#8341=CARTESIAN_POINT('Ctrl Pts',(1.05296815545482,-4.99331396557464,-2.47601943759861));
#8342=CARTESIAN_POINT('Ctrl Pts',(1.1794374382554,-3.3759225189606,-0.508346701513314));
#8343=CARTESIAN_POINT('Ctrl Pts',(1.30590672105597,-4.14151830549257,1.92100234023541));
#8344=CARTESIAN_POINT('Ctrl Pts',(1.43237600385654,-6.59484277307325,2.60582679594369));
#8345=CARTESIAN_POINT('Ctrl Pts',(1.55884528665711,-8.50797749001172,0.924249706642856));
#8346=CARTESIAN_POINT('Ctrl Pts',(1.68531456945769,-8.14355998410671,-1.59666473787506));
#8347=CARTESIAN_POINT('Ctrl Pts',(1.81178385225826,-5.83252664576418,-2.66760869374852));
#8348=CARTESIAN_POINT('Ctrl Pts',(1.93825313505883,-3.67357961447098,-1.31603735411116));
#8349=CARTESIAN_POINT('Ctrl Pts',(2.06472241785941,-3.62730835663665,1.23065841253159));
#8350=CARTESIAN_POINT('Ctrl Pts',(2.19119170065998,-5.73573279288324,2.65976466779286));
#8351=CARTESIAN_POINT('Ctrl Pts',(2.31766098346055,-8.08414435560439,1.67347779933784));
#8352=CARTESIAN_POINT('Ctrl Pts',(2.44413026626113,-8.53989660574529,-0.832532754924229));
#8353=CARTESIAN_POINT('Ctrl Pts',(2.5705995490617,-6.68911047860912,-2.58250116054896));
#8354=CARTESIAN_POINT('Ctrl Pts',(2.69706883186227,-4.2125273137399,-1.98724103946888));
#8355=CARTESIAN_POINT('Ctrl Pts',(2.82353811466284,-3.35918910631978,0.412678277445913));
#8356=CARTESIAN_POINT('Ctrl Pts',(2.95000739746342,-4.90403185928076,2.43783497494159));
#8357=CARTESIAN_POINT('Ctrl Pts',(3.07647668026399,-7.44414842596318,2.24913780421508));
#8358=CARTESIAN_POINT('Ctrl Pts',(3.20294596306457,-8.6728006736903,0.0179469892813684));
#8359=CARTESIAN_POINT('Ctrl Pts',(3.32941524586514,-7.4742213074451,-2.22954189729948));
#8360=CARTESIAN_POINT('Ctrl Pts',(3.45588452866571,-4.93686774870375,-2.45233263496102));
#8361=CARTESIAN_POINT('Ctrl Pts',(3.58235381146628,-3.36496897890566,-0.448103842470657));
#8362=CARTESIAN_POINT('Ctrl Pts',(3.70882309426686,-4.18600233506543,1.9630583300932));
#8363=CARTESIAN_POINT('Ctrl Pts',(3.83529237706743,-6.65436858944041,2.59152219458696));
#8364=CARTESIAN_POINT('Ctrl Pts',(3.961761659868,-8.52848771451476,0.8665652966485));
#8365=CARTESIAN_POINT('Ctrl Pts',(4.08823094266857,-8.1064291347586,-1.64533942882639));
#8366=CARTESIAN_POINT('Ctrl Pts',(4.21470022546916,-5.7714739297676,-2.66307366985099));
#8367=CARTESIAN_POINT('Ctrl Pts',(4.34116950826972,-3.64404849224561,-1.26240961218128));
#8368=CARTESIAN_POINT('Ctrl Pts',(4.4676387910703,-3.65611667168528,1.28467757786444));
#8369=CARTESIAN_POINT('Ctrl Pts',(4.59410807387086,-5.79671907745662,2.66511958500019));
#8370=CARTESIAN_POINT('Ctrl Pts',(4.72057735667144,-8.12192555287883,1.6253053509602));
#8371=CARTESIAN_POINT('Ctrl Pts',(4.84704663947201,-8.52016275023653,-0.890485961787482));
#8372=CARTESIAN_POINT('Ctrl Pts',(4.97351592227259,-6.6297823338236,-2.59760654215074));
#8373=CARTESIAN_POINT('Ctrl Pts',(5.09998520507316,-4.16748213092269,-1.94578102450731));
#8374=CARTESIAN_POINT('Ctrl Pts',(5.22645448787373,-3.36933344852421,0.473052883689435));
#8375=CARTESIAN_POINT('Ctrl Pts',(5.35292377067431,-4.96015341709861,2.46229661492046));
#8376=CARTESIAN_POINT('Ctrl Pts',(5.47939305347488,-7.49528192488301,2.21547229748841));
#8377=CARTESIAN_POINT('Ctrl Pts',(5.60586233627545,-8.67251061031707,-0.043273243038023));
#8378=CARTESIAN_POINT('Ctrl Pts',(5.73233161907603,-7.42277109491315,-2.26272135874042));
#8379=CARTESIAN_POINT('Ctrl Pts',(5.8588009018766,-4.88098050547587,-2.42734029478673));
#8380=CARTESIAN_POINT('Ctrl Pts',(5.98527018467717,-3.3553971927632,-0.387635818488908));
#8381=CARTESIAN_POINT('Ctrl Pts',(6.11173946747774,-4.23143836462047,2.00408963813605));
#8382=CARTESIAN_POINT('Ctrl Pts',(6.23820875027832,-6.71355093380672,2.57585531439246));
#8383=CARTESIAN_POINT('Ctrl Pts',(6.36467803307889,-8.54767152895091,0.808427681609743));
#8384=CARTESIAN_POINT('Ctrl Pts',(6.49114731587946,-8.06819315723838,-1.69315167665925));
#8385=CARTESIAN_POINT('Ctrl Pts',(6.61761659868005,-5.71054112872801,-2.65714115124909));
#8386=CARTESIAN_POINT('Ctrl Pts',(6.74408588148061,-3.61575334229747,-1.20811978340404));
#8387=CARTESIAN_POINT('Ctrl Pts',(6.87055516428119,-3.68615464767176,1.33802287773358));
#8388=CARTESIAN_POINT('Ctrl Pts',(6.99702444708175,-5.85781200422589,2.66907626524016));
#8389=CARTESIAN_POINT('Ctrl Pts',(7.12349372988232,-8.15859354196241,1.57628025947347));
#8390=CARTESIAN_POINT('Ctrl Pts',(7.24996301268291,-8.49910675948999,-0.947972014647327));
#8391=CARTESIAN_POINT('Ctrl Pts',(7.37643229548347,-6.57012379149707,-2.61134915285286));
#8392=CARTESIAN_POINT('Ctrl Pts',(7.50290157828406,-4.12339832812209,-1.90330021301725));
#8393=CARTESIAN_POINT('Ctrl Pts',(7.62937086108461,-3.38085789785896,0.53317931789714));
#8394=CARTESIAN_POINT('Ctrl Pts',(7.7558401438852,-5.01682050197373,2.48546647730356));
#8395=CARTESIAN_POINT('Ctrl Pts',(7.88230942668576,-7.54563096492355,2.18064450472173));
#8396=CARTESIAN_POINT('Ctrl Pts',(8.00877870948635,-8.67081848802445,-0.104470773846832));
#8397=CARTESIAN_POINT('Ctrl Pts',(8.13524799228691,-7.3705744635952,-2.29471374473175));
#8398=CARTESIAN_POINT('Ctrl Pts',(8.26171727508749,-4.82568032696878,-2.40107451829127));
#8399=CARTESIAN_POINT('Ctrl Pts',(8.38818655788806,-3.34721282144588,-0.326964429830057));
#8400=CARTESIAN_POINT('Ctrl Pts',(8.51465584068863,-4.27780222826304,2.04406955140716));
#8401=CARTESIAN_POINT('Ctrl Pts',(8.64112512348922,-6.77235892036706,2.5588370901696));
#8402=CARTESIAN_POINT('Ctrl Pts',(8.76759440628977,-8.56551880203525,0.749865932202442));
#8403=CARTESIAN_POINT('Ctrl Pts',(8.89406368909036,-8.02887211171653,-1.74007563028033));
#8404=CARTESIAN_POINT('Ctrl Pts',(9.02053297189093,-5.64976027465288,-2.64981469118311));
#8405=CARTESIAN_POINT('Ctrl Pts',(9.1470022546915,-3.58870884912087,-1.15319604287949));
#8406=CARTESIAN_POINT('Ctrl Pts',(9.27347153749207,-3.71740685001871,1.3906660199344));
#8407=CARTESIAN_POINT('Ctrl Pts',(9.39994082029265,-5.91897889275454,2.67163307189029));
#8408=CARTESIAN_POINT('Ctrl Pts',(9.52641010309321,-8.19413029627241,1.52642748062739));
#8409=CARTESIAN_POINT('Ctrl Pts',(9.6528793858938,-8.47673736081089,-1.00495933285839));
#8410=CARTESIAN_POINT('Ctrl Pts',(9.77934866869435,-6.51017059021083,-2.62372448418141));
#8411=CARTESIAN_POINT('Ctrl Pts',(9.90581795149495,-4.08029053281044,-1.85981573200689));
#8412=CARTESIAN_POINT('Ctrl Pts',(10.0322872342955,-3.39377267811131,0.593016166654935));
#8413=CARTESIAN_POINT('Ctrl Pts',(10.1587565170961,-5.07397224330304,2.50735129507063));
#8414=CARTESIAN_POINT('Ctrl Pts',(10.2852257998967,-7.59522874000989,2.14463654496994));
#8415=CARTESIAN_POINT('Ctrl Pts',(10.4116950826972,-8.6676110960045,-0.165544298633874));
#8416=CARTESIAN_POINT('Ctrl Pts',(10.5381643654978,-7.31787722698646,-2.32563473540455));
#8417=CARTESIAN_POINT('Ctrl Pts',(10.6646336482984,-4.77057780086958,-2.37329542477909));
#8418=CARTESIAN_POINT('Ctrl Pts',(10.791102931099,-3.34122404818372,-0.266608061508461));
#8419=CARTESIAN_POINT('Ctrl Pts',(10.9175722138995,-4.3235039766914,2.08391767047786));
#8420=CARTESIAN_POINT('Ctrl Pts',(11.0440414967001,-6.83399944658457,2.53859253222465));
#8421=CARTESIAN_POINT('Ctrl Pts',(11.1283543519005,-7.99387663995568,1.30973415156129));
#8422=CARTESIAN_POINT('Ctrl Pts',(11.1705107795007,-8.18769887591545,0.585396224303999));
#8423=CARTESIAN_POINT('Ctrl Pts',(-0.17051077950067,-7.84591438360749,1.55304610346959));
#8424=CARTESIAN_POINT('Ctrl Pts',(-0.128354351900479,-8.3601214382925,0.941871588897895));
#8425=CARTESIAN_POINT('Ctrl Pts',(-0.0440414967000962,-8.7254412199238,
-0.820643964577131));
#8426=CARTESIAN_POINT('Ctrl Pts',(0.0824277861004762,-6.79672120820092,
-2.73529949548601));
#8427=CARTESIAN_POINT('Ctrl Pts',(0.20889706890105,-4.14502274781409,-2.15887236951926));
#8428=CARTESIAN_POINT('Ctrl Pts',(0.335366351701622,-3.17763226925003,0.374524758006143));
#8429=CARTESIAN_POINT('Ctrl Pts',(0.461835634502197,-4.77341883003069,2.56964556571722));
#8430=CARTESIAN_POINT('Ctrl Pts',(0.588304917302768,-7.48302967050217,2.43025383811678));
#8431=CARTESIAN_POINT('Ctrl Pts',(0.714774200103343,-8.84589968864111,0.0843933629786898));
#8432=CARTESIAN_POINT('Ctrl Pts',(0.841243482903914,-7.62432596097212,-2.33836813251456));
#8433=CARTESIAN_POINT('Ctrl Pts',(0.967712765704489,-4.9276734131386,-2.63746727552268));
#8434=CARTESIAN_POINT('Ctrl Pts',(1.09418204850506,-3.20482061667911,-0.541493240926087));
#8435=CARTESIAN_POINT('Ctrl Pts',(1.22065133130563,-4.02033676432878,2.04626051461342));
#8436=CARTESIAN_POINT('Ctrl Pts',(1.34712061410621,-6.63362925356655,2.77573866974455));
#8437=CARTESIAN_POINT('Ctrl Pts',(1.47358989690678,-8.67150913971368,0.98451503193617));
#8438=CARTESIAN_POINT('Ctrl Pts',(1.60005917970735,-8.2833299389138,-1.70077461112773));
#8439=CARTESIAN_POINT('Ctrl Pts',(1.72652846250792,-5.82160661398222,-2.84154903100648));
#8440=CARTESIAN_POINT('Ctrl Pts',(1.8529977453085,-3.52188632174367,-1.40184903322085));
#8441=CARTESIAN_POINT('Ctrl Pts',(1.97946702810907,-3.47259796540763,1.31090299256566));
#8442=CARTESIAN_POINT('Ctrl Pts',(2.10593631090964,-5.71850135738828,2.8331935385365));
#8443=CARTESIAN_POINT('Ctrl Pts',(2.23240559371022,-8.22004013857948,1.78259623694553));
#8444=CARTESIAN_POINT('Ctrl Pts',(2.35887487651079,-8.70550952837483,-0.886817713774895));
#8445=CARTESIAN_POINT('Ctrl Pts',(2.48534415931136,-6.73404364640775,-2.75089209580407));
#8446=CARTESIAN_POINT('Ctrl Pts',(2.61181344211194,-4.0959758860076,-2.11681828122406));
#8447=CARTESIAN_POINT('Ctrl Pts',(2.73828272491251,-3.18699610868948,0.439586796272604));
#8448=CARTESIAN_POINT('Ctrl Pts',(2.86475200771309,-4.83256970350528,2.5967930105464));
#8449=CARTESIAN_POINT('Ctrl Pts',(2.99122129051365,-7.53831353528048,2.3957919177369));
#8450=CARTESIAN_POINT('Ctrl Pts',(3.11769057331423,-8.84707955188353,0.0191172154002425));
#8451=CARTESIAN_POINT('Ctrl Pts',(3.2441598561148,-7.57034730673834,-2.37491826770037));
#8452=CARTESIAN_POINT('Ctrl Pts',(3.37062913891538,-4.86754664371048,-2.61223598457652));
#8453=CARTESIAN_POINT('Ctrl Pts',(3.49709842171595,-3.19315285551078,-0.477322270821332));
#8454=CARTESIAN_POINT('Ctrl Pts',(3.62356770451652,-4.06772135691324,2.09105874814314));
#8455=CARTESIAN_POINT('Ctrl Pts',(3.7500369873171,-6.69703642652049,2.76050134268853));
#8456=CARTESIAN_POINT('Ctrl Pts',(3.87650627011767,-8.69335672504318,0.923069333506797));
#8457=CARTESIAN_POINT('Ctrl Pts',(4.00297555291824,-8.24377798767264,-1.75262311545725));
#8458=CARTESIAN_POINT('Ctrl Pts',(4.12944483571881,-5.75657298053108,-2.83671830272471));
#8459=CARTESIAN_POINT('Ctrl Pts',(4.25591411851939,-3.4904296347338,-1.34472451624315));
#8460=CARTESIAN_POINT('Ctrl Pts',(4.38238340131996,-3.50328471489348,1.36844445554975));
#8461=CARTESIAN_POINT('Ctrl Pts',(4.50885268412054,-5.78346422778239,2.83889762093706));
#8462=CARTESIAN_POINT('Ctrl Pts',(4.63532196692111,-8.26028484341833,1.73128272371194));
#8463=CARTESIAN_POINT('Ctrl Pts',(4.76179124972168,-8.68448893486336,-0.94854973586341));
#8464=CARTESIAN_POINT('Ctrl Pts',(4.88826053252225,-6.67084703413032,-2.76698241765453));
#8465=CARTESIAN_POINT('Ctrl Pts',(5.01472981532283,-4.04799355041029,-2.07265488289069));
#8466=CARTESIAN_POINT('Ctrl Pts',(5.1411990981234,-3.19780190859137,0.503898104100741));
#8467=CARTESIAN_POINT('Ctrl Pts',(5.26766838092397,-4.89235064461916,2.62284966178678));
#8468=CARTESIAN_POINT('Ctrl Pts',(5.39413766372455,-7.59278117314959,2.35993126536998));
#8469=CARTESIAN_POINT('Ctrl Pts',(5.52060694652512,-8.84677057504632,-0.0460948572072665));
#8470=CARTESIAN_POINT('Ctrl Pts',(5.64707622932569,-7.51554230407514,-2.41026118239688));
#8471=CARTESIAN_POINT('Ctrl Pts',(5.77354551212627,-4.80801529557386,-2.58561402905087));
#8472=CARTESIAN_POINT('Ctrl Pts',(5.90001479492683,-3.18295694495545,-0.412911453989435));
#8473=CARTESIAN_POINT('Ctrl Pts',(6.02648407772741,-4.11612002425056,2.13476548589794));
#8474=CARTESIAN_POINT('Ctrl Pts',(6.15295336052799,-6.76007773152183,2.74381290995853));
#8475=CARTESIAN_POINT('Ctrl Pts',(6.27942264332856,-8.71379141227815,0.861140878982882));
#8476=CARTESIAN_POINT('Ctrl Pts',(6.40589192612912,-8.20304884882752,-1.8035529414164));
#8477=CARTESIAN_POINT('Ctrl Pts',(6.53236120892971,-5.69166708104277,-2.83039895666613));
#8478=CARTESIAN_POINT('Ctrl Pts',(6.65883049173027,-3.46028951106959,-1.28689474131513));
#8479=CARTESIAN_POINT('Ctrl Pts',(6.78529977453086,-3.5352813048573,1.42526811394729));
#8480=CARTESIAN_POINT('Ctrl Pts',(6.91176905733142,-5.84854069393329,2.84311229489889));
#8481=CARTESIAN_POINT('Ctrl Pts',(7.03823834013199,-8.2993437537801,1.67906097112298));
#8482=CARTESIAN_POINT('Ctrl Pts',(7.16470762293257,-8.662059996825,-1.00978414336219));
#8483=CARTESIAN_POINT('Ctrl Pts',(7.29117690573314,-6.60729848087495,-2.78162110968445));
#8484=CARTESIAN_POINT('Ctrl Pts',(7.41764618853372,-4.00103528122159,-2.02740412740739));
#8485=CARTESIAN_POINT('Ctrl Pts',(7.54411547133428,-3.21007780494632,0.567945057936651));
#8486=CARTESIAN_POINT('Ctrl Pts',(7.67058475413486,-4.95271268365969,2.64753030559991));
#8487=CARTESIAN_POINT('Ctrl Pts',(7.79705403693543,-7.64641320181803,2.32283254057568));
#8488=CARTESIAN_POINT('Ctrl Pts',(7.92352331973601,-8.8449681186095,-0.111282748061457));
#8489=CARTESIAN_POINT('Ctrl Pts',(8.04999260253658,-7.45994221269332,-2.44433961887307));
#8490=CARTESIAN_POINT('Ctrl Pts',(8.17646188533714,-4.7491092914738,-2.55763560330791));
#8491=CARTESIAN_POINT('Ctrl Pts',(8.30293116813774,-3.17423891504325,-0.34828401216958));
#8492=CARTESIAN_POINT('Ctrl Pts',(8.42940045093828,-4.16550702471881,2.17735227311358));
#8493=CARTESIAN_POINT('Ctrl Pts',(8.55586973373889,-6.82272026886908,2.72568501936376));
#8494=CARTESIAN_POINT('Ctrl Pts',(8.68233901653944,-8.73280240952739,0.798760634581848));
#8495=CARTESIAN_POINT('Ctrl Pts',(8.80880829934001,-8.16116389056411,-1.85353655230184));
#8496=CARTESIAN_POINT('Ctrl Pts',(8.93527758214061,-5.62692303615881,-2.82259477775864));
#8497=CARTESIAN_POINT('Ctrl Pts',(9.06174686494115,-3.43148159274178,-1.22838972068279));
#8498=CARTESIAN_POINT('Ctrl Pts',(9.18821614774175,-3.56857129431638,1.48134383077204));
#8499=CARTESIAN_POINT('Ctrl Pts',(9.3146854305423,-5.91369594448993,2.84583581708419));
#8500=CARTESIAN_POINT('Ctrl Pts',(9.44115471334289,-8.33719766766608,1.62595756215785));
#8501=CARTESIAN_POINT('Ctrl Pts',(9.56762399614346,-8.63823201062531,-1.07048729642275));
#8502=CARTESIAN_POINT('Ctrl Pts',(9.69409327894403,-6.54343605554251,-2.7948033694467));
#8503=CARTESIAN_POINT('Ctrl Pts',(9.8205625617446,-3.95511665969225,-1.98108425854193));
#8504=CARTESIAN_POINT('Ctrl Pts',(9.94703184454517,-3.22383468817951,0.631683544021454));
#8505=CARTESIAN_POINT('Ctrl Pts',(10.0735011273458,-5.01359098098088,2.67084211398678));
#8506=CARTESIAN_POINT('Ctrl Pts',(10.1999704101463,-7.69924497960724,2.28447669648917));
#8507=CARTESIAN_POINT('Ctrl Pts',(10.3264396929469,-8.84155158990058,-0.176338547131783));
#8508=CARTESIAN_POINT('Ctrl Pts',(10.4529089757475,-7.40380887425685,-2.47727680013581));
#8509=CARTESIAN_POINT('Ctrl Pts',(10.579378258548,-4.69041382762631,-2.52804518532915));
#8510=CARTESIAN_POINT('Ctrl Pts',(10.7058475413486,-3.16785964626223,-0.283992131459634));
#8511=CARTESIAN_POINT('Ctrl Pts',(10.8323168241492,-4.21418873702027,2.2197986725417));
#8512=CARTESIAN_POINT('Ctrl Pts',(10.9587861069498,-6.88838004046696,2.70412042327197));
#8513=CARTESIAN_POINT('Ctrl Pts',(11.0430989621501,-8.12388655333519,1.39513483291862));
#8514=CARTESIAN_POINT('Ctrl Pts',(11.0852553897503,-8.33034688916693,0.623566746436274));
#8515=CARTESIAN_POINT('Ctrl Pts',(-0.255766169251004,-7.95890872821688,
1.64811304057572));
#8516=CARTESIAN_POINT('Ctrl Pts',(-0.213609741650813,-8.50459204726909,
0.999526572161923));
#8517=CARTESIAN_POINT('Ctrl Pts',(-0.129296886450431,-8.89227422537169,
-0.87087821582871));
#8518=CARTESIAN_POINT('Ctrl Pts',(-0.00282760364985846,-6.84549107074519,
-2.90273595762506));
#8519=CARTESIAN_POINT('Ctrl Pts',(0.123641679150715,-4.03147363592819,-2.29102387700814));
#8520=CARTESIAN_POINT('Ctrl Pts',(0.250110961951288,-3.0048660809507,0.397450620628325));
#8521=CARTESIAN_POINT('Ctrl Pts',(0.376580244751861,-4.69833585942183,2.72694181908363));
#8522=CARTESIAN_POINT('Ctrl Pts',(0.503049527552434,-7.57381067700105,2.57901747640416));
#8523=CARTESIAN_POINT('Ctrl Pts',(0.629518810353007,-9.02010634361806,0.0895593516203334));
#8524=CARTESIAN_POINT('Ctrl Pts',(0.755988093153582,-7.72375616695671,-2.48150715181869));
#8525=CARTESIAN_POINT('Ctrl Pts',(0.882457375954152,-4.86203286070258,-2.79891511344676));
#8526=CARTESIAN_POINT('Ctrl Pts',(1.00892665875473,-3.03371871439761,-0.574639780338865));
#8527=CARTESIAN_POINT('Ctrl Pts',(1.1353959415553,-3.899155223165,2.17151868899145));
#8528=CARTESIAN_POINT('Ctrl Pts',(1.26186522435587,-6.67241573405984,2.94565054354541));
#8529=CARTESIAN_POINT('Ctrl Pts',(1.38833450715645,-8.83504078941567,1.04478035722949));
#8530=CARTESIAN_POINT('Ctrl Pts',(1.51480378995702,-8.42309989372086,-1.8048844843804));
#8531=CARTESIAN_POINT('Ctrl Pts',(1.64127307275759,-5.81068658220031,-3.01548936826444));
#8532=CARTESIAN_POINT('Ctrl Pts',(1.76774235555817,-3.37019302901635,-1.48766071233055));
#8533=CARTESIAN_POINT('Ctrl Pts',(1.89421163835874,-3.31788757417861,1.39114757259974));
#8534=CARTESIAN_POINT('Ctrl Pts',(2.02068092115931,-5.70126992189332,3.00662240928013));
#8535=CARTESIAN_POINT('Ctrl Pts',(2.14715020395988,-8.35593592155457,1.89171467455323));
#8536=CARTESIAN_POINT('Ctrl Pts',(2.27361948676046,-8.87112245100439,-0.941102672625564));
#8537=CARTESIAN_POINT('Ctrl Pts',(2.40008876956103,-6.77897681420636,-2.91928303105917));
#8538=CARTESIAN_POINT('Ctrl Pts',(2.5265580523616,-3.9794244582753,-2.24639552297924));
#8539=CARTESIAN_POINT('Ctrl Pts',(2.65302733516218,-3.01480311105916,0.466495315099294));
#8540=CARTESIAN_POINT('Ctrl Pts',(2.77949661796275,-4.7611075477298,2.75575104615122));
#8541=CARTESIAN_POINT('Ctrl Pts',(2.90596590076332,-7.63247864459777,2.54244603125873));
#8542=CARTESIAN_POINT('Ctrl Pts',(3.03243518356389,-9.02135843007676,0.0202874415191203));
#8543=CARTESIAN_POINT('Ctrl Pts',(3.15890446636447,-7.66647330603156,-2.52029463810126));
#8544=CARTESIAN_POINT('Ctrl Pts',(3.28537374916504,-4.79822553871722,-2.77213933419203));
#8545=CARTESIAN_POINT('Ctrl Pts',(3.41184303196562,-3.02133673211591,-0.506540699172009));
#8546=CARTESIAN_POINT('Ctrl Pts',(3.53831231476618,-3.94944037876103,2.21905916619308));
#8547=CARTESIAN_POINT('Ctrl Pts',(3.66478159756677,-6.73970426360059,2.92948049079009));
#8548=CARTESIAN_POINT('Ctrl Pts',(3.79125088036733,-8.85822573557158,0.979573370365098));
#8549=CARTESIAN_POINT('Ctrl Pts',(3.91772016316791,-8.3811268405867,-1.85990680208812));
#8550=CARTESIAN_POINT('Ctrl Pts',(4.04418944596848,-5.74167203129455,-3.01036293559842));
#8551=CARTESIAN_POINT('Ctrl Pts',(4.17065872876906,-3.336810777222,-1.42703942030501));
#8552=CARTESIAN_POINT('Ctrl Pts',(4.29712801156963,-3.3504527581017,1.45221133323505));
#8553=CARTESIAN_POINT('Ctrl Pts',(4.4235972943702,-5.77020937810816,3.01267565687393));
#8554=CARTESIAN_POINT('Ctrl Pts',(4.55006657717077,-8.39864413395782,1.83726009646369));
#8555=CARTESIAN_POINT('Ctrl Pts',(4.67653585997135,-8.84881511949022,-1.00661350993934));
#8556=CARTESIAN_POINT('Ctrl Pts',(4.80300514277192,-6.71191173443704,-2.93635829315832));
#8557=CARTESIAN_POINT('Ctrl Pts',(4.92947442557249,-3.92850496989789,-2.19952874127408));
#8558=CARTESIAN_POINT('Ctrl Pts',(5.05594370837306,-3.02627036865852,0.534743324512047));
#8559=CARTESIAN_POINT('Ctrl Pts',(5.18241299117364,-4.82454787213973,2.7834027086531));
#8560=CARTESIAN_POINT('Ctrl Pts',(5.3088822739742,-7.69028042141618,2.50439023325154));
#8561=CARTESIAN_POINT('Ctrl Pts',(5.43535155677479,-9.02103053977556,-0.0489164713765121));
#8562=CARTESIAN_POINT('Ctrl Pts',(5.56182083957535,-7.60831351323712,-2.55780100605334));
#8563=CARTESIAN_POINT('Ctrl Pts',(5.68829012237593,-4.73505008567186,-2.743887763315));
#8564=CARTESIAN_POINT('Ctrl Pts',(5.81475940517651,-3.01051669714769,-0.438187089489962));
#8565=CARTESIAN_POINT('Ctrl Pts',(5.94122868797708,-4.00080168388066,2.26544133365983));
#8566=CARTESIAN_POINT('Ctrl Pts',(6.06769797077765,-6.80660452923693,2.9117705055246));
#8567=CARTESIAN_POINT('Ctrl Pts',(6.19416725357822,-8.87991129560537,0.913854076356023));
#8568=CARTESIAN_POINT('Ctrl Pts',(6.32063653637879,-8.33790454041667,-1.91395420617355));
#8569=CARTESIAN_POINT('Ctrl Pts',(6.44710581917937,-5.67279303335752,-3.00365676208316));
#8570=CARTESIAN_POINT('Ctrl Pts',(6.57357510197994,-3.30482567984171,-1.36566969922623));
#8571=CARTESIAN_POINT('Ctrl Pts',(6.70004438478051,-3.38440796204285,1.51251335016101));
#8572=CARTESIAN_POINT('Ctrl Pts',(6.8265136675811,-5.83926938364069,3.01714832455762));
#8573=CARTESIAN_POINT('Ctrl Pts',(6.95298295038165,-8.44009396559778,1.78184168277249));
#8574=CARTESIAN_POINT('Ctrl Pts',(7.07945223318224,-8.82501323416001,-1.07159627207705));
#8575=CARTESIAN_POINT('Ctrl Pts',(7.2059215159828,-6.6444731702528,-2.95189306651605));
#8576=CARTESIAN_POINT('Ctrl Pts',(7.33239079878339,-3.87867223432111,-2.15150804179754));
#8577=CARTESIAN_POINT('Ctrl Pts',(7.45886008158394,-3.03929771203367,0.602710797976159));
#8578=CARTESIAN_POINT('Ctrl Pts',(7.58532936438453,-4.88860486534565,2.80959413389628));
#8579=CARTESIAN_POINT('Ctrl Pts',(7.7117986471851,-7.74719543871252,2.46502057642963));
#8580=CARTESIAN_POINT('Ctrl Pts',(7.83826792998567,-9.01911774919456,-0.118094722276079));
#8581=CARTESIAN_POINT('Ctrl Pts',(7.96473721278625,-7.54930996179144,-2.5939654930144));
#8582=CARTESIAN_POINT('Ctrl Pts',(8.09120649558682,-4.67253825597884,-2.71419668832455));
#8583=CARTESIAN_POINT('Ctrl Pts',(8.21767577838739,-3.00126500864061,-0.369603594509102));
#8584=CARTESIAN_POINT('Ctrl Pts',(8.34414506118797,-4.05321182117459,2.31063499481999));
#8585=CARTESIAN_POINT('Ctrl Pts',(8.47061434398855,-6.87308161737107,2.89253294855792));
#8586=CARTESIAN_POINT('Ctrl Pts',(8.59708362678911,-8.90008601701954,0.847655336961254));
#8587=CARTESIAN_POINT('Ctrl Pts',(8.72355290958969,-8.29345566941167,-1.96699747432336));
#8588=CARTESIAN_POINT('Ctrl Pts',(8.85002219239025,-5.60408579766473,-2.99537486433416));
#8589=CARTESIAN_POINT('Ctrl Pts',(8.97649147519084,-3.27425433636271,-1.30358339848609));
#8590=CARTESIAN_POINT('Ctrl Pts',(9.1029607579914,-3.41973573861403,1.57202164160968));
#8591=CARTESIAN_POINT('Ctrl Pts',(9.22943004079198,-5.90841299622533,3.0200385622781));
#8592=CARTESIAN_POINT('Ctrl Pts',(9.35589932359255,-8.48026503905977,1.72548764368831));
#8593=CARTESIAN_POINT('Ctrl Pts',(9.48236860639313,-8.79972666043973,-1.1360152599871));
#8594=CARTESIAN_POINT('Ctrl Pts',(9.60883788919369,-6.57670152087419,-2.96588225471199));
#8595=CARTESIAN_POINT('Ctrl Pts',(9.73530717199427,-3.82994278657406,-2.10235278507697));
#8596=CARTESIAN_POINT('Ctrl Pts',(9.86177645479484,-3.0538966982477,0.670350921387973));
#8597=CARTESIAN_POINT('Ctrl Pts',(9.98824573759542,-4.95320971865872,2.83433293290292));
#8598=CARTESIAN_POINT('Ctrl Pts',(10.114715020396,-7.80326121920459,2.4243168480084));
#8599=CARTESIAN_POINT('Ctrl Pts',(10.2411843031966,-9.01549208379667,-0.187132795629694));
#8600=CARTESIAN_POINT('Ctrl Pts',(10.3676535859971,-7.48974052152724,-2.62891886486708));
#8601=CARTESIAN_POINT('Ctrl Pts',(10.4941228687977,-4.61024985438304,-2.68279494587922));
#8602=CARTESIAN_POINT('Ctrl Pts',(10.6205921515983,-2.99449524434074,-0.301376201410799));
#8603=CARTESIAN_POINT('Ctrl Pts',(10.7470614343989,-4.10487349734913,2.35567967460553));
#8604=CARTESIAN_POINT('Ctrl Pts',(10.8735307171994,-6.94276063434935,2.8696483143193));
#8605=CARTESIAN_POINT('Ctrl Pts',(10.9578435723998,-8.2538964667147,1.48053551427594));
#8606=CARTESIAN_POINT('Ctrl Pts',(11.,-8.47299490241841,0.661737268568548));
#8607=CARTESIAN_POINT('Ctrl Pts',(-2.77555756156289E-16,-7.61992569438872,
1.36291222925734));
#8608=CARTESIAN_POINT('Ctrl Pts',(-2.8415648060146E-16,-7.67340551349811,
1.31130789569533));
#8609=CARTESIAN_POINT('Ctrl Pts',(-2.12884066448237E-16,-7.72375637073556,
1.25685433110144));
#8610=CARTESIAN_POINT('Ctrl Pts',(-2.20309881449055E-16,-7.77098328294997,
1.19991834123266));
#8611=CARTESIAN_POINT('Ctrl Pts',(-2.2794194360023E-16,-7.81952189173417,
1.14140099151826));
#8612=CARTESIAN_POINT('Ctrl Pts',(-5.34217411271648E-16,-7.86476106583717,
1.08026093410145));
#8613=CARTESIAN_POINT('Ctrl Pts',(-5.30825383648903E-16,-7.90667917618666,
1.01684878351049));
#8614=CARTESIAN_POINT('Ctrl Pts',(-5.27540844822369E-16,-7.94726895796044,
0.955446078740799));
#8615=CARTESIAN_POINT('Ctrl Pts',(-1.29049571234523E-16,-7.98474497647301,
0.891912164254134));
#8616=CARTESIAN_POINT('Ctrl Pts',(-1.87350135405495E-16,-8.01905850567605,
0.826531736936219));
#8617=CARTESIAN_POINT('Ctrl Pts',(-2.12856632230295E-16,-8.03407067470238,
0.797927799984632));
#8618=CARTESIAN_POINT('Ctrl Pts',(-1.8986486044456E-16,-8.04847712697053,
0.76897005896662));
#8619=CARTESIAN_POINT('Ctrl Pts',(-1.87350135405495E-16,-8.06227182896166,
0.739680838297154));
#8620=CARTESIAN_POINT('Ctrl Pts',(-1.85669547491645E-16,-8.07149081277949,
0.720106885082177));
#8621=CARTESIAN_POINT('Ctrl Pts',(-1.91431563196273E-16,-8.08043654946019,
0.70038486767912));
#8622=CARTESIAN_POINT('Ctrl Pts',(-1.87350135405495E-16,-8.08910691796322,
0.680521268938271));
#8623=CARTESIAN_POINT('Ctrl Pts',(-1.84817515006514E-16,-8.09448708227411,
0.668195446224487));
#8624=CARTESIAN_POINT('Ctrl Pts',(-5.32249335375699E-16,-8.09975758272891,
0.65582334914044));
#8625=CARTESIAN_POINT('Ctrl Pts',(-5.13478148889135E-16,-8.1049165612927,
0.643411087671161));
#8626=CARTESIAN_POINT('Ctrl Pts',(-4.01571461942795E-16,-8.13567243277232,
0.569413897374587));
#8627=CARTESIAN_POINT('Ctrl Pts',(7.11652356572681E-17,-8.16248855621688,
0.493944535414431));
#8628=CARTESIAN_POINT('Ctrl Pts',(6.93889390390723E-17,-8.1853403815105,
0.417382497740407));
#8629=CARTESIAN_POINT('Ctrl Pts',(6.75847180162072E-17,-8.20855145064346,
0.33961686079112));
#8630=CARTESIAN_POINT('Ctrl Pts',(-3.39859180694956E-18,-8.22767309653215,
0.260723103319841));
#8631=CARTESIAN_POINT('Ctrl Pts',(-2.77555756156289E-17,-8.24263877411456,
0.181064199295853));
#8632=CARTESIAN_POINT('Ctrl Pts',(-4.9418863841957E-17,-8.25594936254853,
0.110214959044269));
#8633=CARTESIAN_POINT('Ctrl Pts',(-2.34406229728529E-16,-8.26597201859407,
0.0387595244952337));
#8634=CARTESIAN_POINT('Ctrl Pts',(-1.94289029309402E-16,-8.27262867129198,
-0.033060966067791));
#8635=CARTESIAN_POINT('Ctrl Pts',(-1.78758283697696E-16,-8.27520569009181,
-0.0608651437518981));
#8636=CARTESIAN_POINT('Ctrl Pts',(1.70471564310096E-16,-8.27727790351381,
-0.0887241302716296));
#8637=CARTESIAN_POINT('Ctrl Pts',(1.80411241501588E-16,-8.27883947623463,
-0.116624198769123));
#8638=CARTESIAN_POINT('Ctrl Pts',(1.85936496667142E-16,-8.27970752130047,
-0.132133253501507));
#8639=CARTESIAN_POINT('Ctrl Pts',(-2.39785655553094E-16,-8.28041776438053,
-0.147655004235494));
#8640=CARTESIAN_POINT('Ctrl Pts',(-2.4980018054066E-16,-8.28096910004911,
-0.163187100078598));
#8641=CARTESIAN_POINT('Ctrl Pts',(-2.58342787073613E-16,-8.28143940130555,
-0.176436313953894));
#8642=CARTESIAN_POINT('Ctrl Pts',(-9.71445146547012E-17,-8.28179374468433,
-0.189684521305536));
#8643=CARTESIAN_POINT('Ctrl Pts',(-9.71445146547012E-17,-8.28203184796289,
-0.202925957134301));
#8644=CARTESIAN_POINT('Ctrl Pts',(-9.71445146547012E-17,-8.2835319015313,
-0.286347164882211));
#8645=CARTESIAN_POINT('Ctrl Pts',(3.42590742071393E-16,-8.28042407041806,
-0.369551099405944));
#8646=CARTESIAN_POINT('Ctrl Pts',(2.4980018054066E-16,-8.27264922864484,
-0.452158464222489));
#8647=CARTESIAN_POINT('Ctrl Pts',(1.64944085125772E-16,-8.26553920899994,
-0.527702122060185));
#8648=CARTESIAN_POINT('Ctrl Pts',(-1.23009909160896E-16,-8.25452592361271,
-0.602747787578086));
#8649=CARTESIAN_POINT('Ctrl Pts',(-1.94289029309402E-16,-8.23952773590921,
-0.677016823098132));
#8650=CARTESIAN_POINT('Ctrl Pts',(-2.70259366732582E-16,-8.22354244627324,
-0.756173856417238));
#8651=CARTESIAN_POINT('Ctrl Pts',(-1.27582757010408E-16,-8.20303136853968,
-0.834449499034265));
#8652=CARTESIAN_POINT('Ctrl Pts',(-8.32667268468867E-17,-8.17825979510907,
-0.911615546253567));
#8653=CARTESIAN_POINT('Ctrl Pts',(-6.63256748201779E-17,-8.16879016272722,
-0.941114443510699));
#8654=CARTESIAN_POINT('Ctrl Pts',(1.29856532866623E-17,-8.15869737053701,
-0.970451130557648));
#8655=CARTESIAN_POINT('Ctrl Pts',(5.55111512312578E-17,-8.14799429148353,
-0.999612516884173));
#8656=CARTESIAN_POINT('Ctrl Pts',(7.48427287796255E-17,-8.1431288010665,
-1.01286893076376));
#8657=CARTESIAN_POINT('Ctrl Pts',(-2.0843408605211E-16,-8.1381371807216,
-1.02608911501842));
#8658=CARTESIAN_POINT('Ctrl Pts',(-1.94289029309402E-16,-8.1330205709451,
-1.03927181904394));
#8659=CARTESIAN_POINT('Ctrl Pts',(-1.81761449722105E-16,-8.12848904184923,
-1.05094709026127));
#8660=CARTESIAN_POINT('Ctrl Pts',(-3.0517213644317E-16,-8.12386085858254,
-1.062589268253));
#8661=CARTESIAN_POINT('Ctrl Pts',(-3.05311331771918E-16,-8.11914027396792,
-1.07418977377208));
#8662=CARTESIAN_POINT('Ctrl Pts',(-3.06245451009502E-16,-8.08746112969757,
-1.15203904837463));
#8663=CARTESIAN_POINT('Ctrl Pts',(1.46916949704505E-16,-8.05158497707301,
-1.22811622682948));
#8664=CARTESIAN_POINT('Ctrl Pts',(1.66533453693773E-16,-8.011854620096,
-1.30218190876206));
#8665=CARTESIAN_POINT('Ctrl Pts',(1.8637260655645E-16,-7.97167332042167,
-1.37708824204871));
#8666=CARTESIAN_POINT('Ctrl Pts',(3.72027912645227E-17,-7.92754941417975,
-1.44993793701178));
#8667=CARTESIAN_POINT('Ctrl Pts',(2.77555756156289E-17,-7.87978125494087,
-1.52047793744191));
#8668=CARTESIAN_POINT('Ctrl Pts',(1.82162073883537E-17,-7.83154714264218,
-1.59170601816577));
#8669=CARTESIAN_POINT('Ctrl Pts',(-2.18320265390652E-16,-7.77959686600608,
-1.66057998181683));
#8670=CARTESIAN_POINT('Ctrl Pts',(-2.4980018054066E-16,-7.72418728444125,
-1.72682140823545));
#8671=CARTESIAN_POINT('Ctrl Pts',(-2.62655382569273E-16,-7.70156011527822,
-1.75387189154257));
#8672=CARTESIAN_POINT('Ctrl Pts',(-7.7813004774142E-17,-7.67835553557515,
-1.78048309521614));
#8673=CARTESIAN_POINT('Ctrl Pts',(-8.32667268468867E-17,-7.65458894362178,
-1.80663469511614));
#8674=CARTESIAN_POINT('Ctrl Pts',(-8.66440684510765E-17,-7.63987094026128,
-1.82282966896707));
#8675=CARTESIAN_POINT('Ctrl Pts',(-2.43913607355091E-17,-7.62493270407027,
-1.8388530693696));
#8676=CARTESIAN_POINT('Ctrl Pts',(-5.55111512312578E-17,-7.60980251222269,
-1.85467449041822));
#8677=CARTESIAN_POINT('Ctrl Pts',(-1.84813850145164E-16,-7.54693657997148,
-1.92041247932014));
#8678=CARTESIAN_POINT('Ctrl Pts',(-7.96394343888385E-17,-7.48070447872273,
-1.98273188781124));
#8679=CARTESIAN_POINT('Ctrl Pts',(-1.38777878078145E-16,-7.41143126172467,
-2.04132873838597));
#8680=CARTESIAN_POINT('Ctrl Pts',(-1.83131710845124E-16,-7.35947634897613,
-2.08527637631701));
#8681=CARTESIAN_POINT('Ctrl Pts',(-3.08318371281544E-16,-7.30580954729488,
-2.12712980226528));
#8682=CARTESIAN_POINT('Ctrl Pts',(-3.05311331771918E-16,-7.25055002523813,
-2.1667490967338));
#8683=CARTESIAN_POINT('Ctrl Pts',(-3.04270587907503E-16,-7.2314245670102,
-2.18046143323572));
#8684=CARTESIAN_POINT('Ctrl Pts',(-5.15303059498705E-16,-7.21210820012051,
-2.19390604239713));
#8685=CARTESIAN_POINT('Ctrl Pts',(-5.55111512312578E-16,-7.19260549845642,
-2.20707675358934));
#8686=CARTESIAN_POINT('Ctrl Pts',(-5.87305517585258E-16,-7.17683321805303,
-2.21772820863456));
#8687=CARTESIAN_POINT('Ctrl Pts',(-8.35843188115225E-16,-7.16094634262041,
-2.22819555243348));
#8688=CARTESIAN_POINT('Ctrl Pts',(-8.04911692853238E-16,-7.14495254626684,
-2.23847286770512));
#8689=CARTESIAN_POINT('Ctrl Pts',(-6.6023125743896E-16,-7.07014240854922,
-2.28654446708293));
#8690=CARTESIAN_POINT('Ctrl Pts',(6.61429474879476E-17,-6.99296303382602,
-2.33048352074413));
#8691=CARTESIAN_POINT('Ctrl Pts',(1.66533453693773E-16,-6.91368947490656,
-2.36999461204078));
#8692=CARTESIAN_POINT('Ctrl Pts',(2.48179831249947E-16,-6.84921725371376,
-2.40212850198302));
#8693=CARTESIAN_POINT('Ctrl Pts',(-6.79181988010686E-17,-6.78335891798408,
-2.43133326054258));
#8694=CARTESIAN_POINT('Ctrl Pts',(-5.55111512312578E-17,-6.71624580957888,
-2.4574306487719));
#8695=CARTESIAN_POINT('Ctrl Pts',(3.78536928224624E-18,-6.69861361567082,
-2.4642870471818));
#8696=CARTESIAN_POINT('Ctrl Pts',(-6.28715915022922E-17,-6.68089474419301,
-2.47092885494305));
#8697=CARTESIAN_POINT('Ctrl Pts',(-5.55111512312578E-17,-6.66309273064558,
-2.4773571349477));
#8698=CARTESIAN_POINT('Ctrl Pts',(1.2890562790225,-3.88215585431528,-0.00180833227560233));
#8699=CARTESIAN_POINT('Ctrl Pts',(1.28093512868358,-3.88093924960685,-0.136660466501262));
#8700=CARTESIAN_POINT('Ctrl Pts',(1.27281397834465,-3.89272649643071,-0.271300596775523));
#8701=CARTESIAN_POINT('Ctrl Pts',(1.26469282800573,-3.91829200827257,-0.403271347036546));
#8702=CARTESIAN_POINT('Ctrl Pts',(1.22253640040554,-4.05100112016495,-1.0883239746252));
#8703=CARTESIAN_POINT('Ctrl Pts',(1.18037997280535,-4.55497781908782,-1.70144778714986));
#8704=CARTESIAN_POINT('Ctrl Pts',(1.13822354520516,-5.20138467371462,-1.96426277578416));
#8705=CARTESIAN_POINT('Ctrl Pts',(1.09606711760497,-5.84779152834142,-2.22707776441846));
#8706=CARTESIAN_POINT('Ctrl Pts',(1.05391069000478,-6.63662853867215,-2.13958392916239));
#8707=CARTESIAN_POINT('Ctrl Pts',(1.01175426240459,-7.20971718211825,-1.74147843160073));
#8708=CARTESIAN_POINT('Ctrl Pts',(0.969597834804394,-7.78280582556434,-1.34337293403907));
#8709=CARTESIAN_POINT('Ctrl Pts',(0.927441407204202,-8.14014610212581,-0.634655774171833));
#8710=CARTESIAN_POINT('Ctrl Pts',(0.885284979604011,-8.11947978687606,0.0628136684028912));
#8711=CARTESIAN_POINT('Ctrl Pts',(0.843128552003819,-8.09881347162631,0.760283110977616));
#8712=CARTESIAN_POINT('Ctrl Pts',(0.800972124403629,-7.70014056456535,1.44650483625982));
#8713=CARTESIAN_POINT('Ctrl Pts',(0.758815696803438,-7.10449029665888,1.81000344847466));
#8714=CARTESIAN_POINT('Ctrl Pts',(0.716659269203247,-6.50884002875241,2.17350206068949));
#8715=CARTESIAN_POINT('Ctrl Pts',(0.674502841603055,-5.71621240000042,2.21427755983694));
#8716=CARTESIAN_POINT('Ctrl Pts',(0.632346414002864,-5.08649523139113,1.91360197170689));
#8717=CARTESIAN_POINT('Ctrl Pts',(0.590189986402673,-4.45677806278185,1.61292638357685));
#8718=CARTESIAN_POINT('Ctrl Pts',(0.548033558802483,-3.98997135431527,0.970799708169316));
#8719=CARTESIAN_POINT('Ctrl Pts',(0.505877131202292,-3.89806072103819,0.27919597258167));
#8720=CARTESIAN_POINT('Ctrl Pts',(0.500270180475695,-3.88583628881346,0.187210282889286));
#8721=CARTESIAN_POINT('Ctrl Pts',(0.494663229749097,-3.88024373829367,0.0943493479437828));
#8722=CARTESIAN_POINT('Ctrl Pts',(0.4890562790225,-3.88098062526521,0.00140302826277638));
#8723=CARTESIAN_POINT('Ctrl Pts',(0.,-5.33826273143149,-2.47299490241842));
#8724=CARTESIAN_POINT('Ctrl Pts',(0.042156427600191,-4.51946448572409,-2.25389646671472));
#8725=CARTESIAN_POINT('Ctrl Pts',(0.126469282800573,-3.13035187791014,-0.942759478034699));
#8726=CARTESIAN_POINT('Ctrl Pts',(0.252938565601146,-3.64432015505377,1.8951258406221));
#8727=CARTESIAN_POINT('Ctrl Pts',(0.379407848401719,-6.30137623450992,3.00550525361278));
#8728=CARTESIAN_POINT('Ctrl Pts',(0.505877131202293,-8.68279501755112,1.3897499208415));
#8729=CARTESIAN_POINT('Ctrl Pts',(0.632346414002865,-8.62891891149828,-1.48974040295355));
#8730=CARTESIAN_POINT('Ctrl Pts',(0.758815696803439,-6.18713281460021,-3.01549224619728));
#8731=CARTESIAN_POINT('Ctrl Pts',(0.88528497960401,-3.57568308349712,-1.80326120932383));
#8732=CARTESIAN_POINT('Ctrl Pts',(1.01175426240459,-3.16566700707563,1.04679027585758));
#8733=CARTESIAN_POINT('Ctrl Pts',(1.13822354520516,-5.32964905792872,2.94610338914275));
#8734=CARTESIAN_POINT('Ctrl Pts',(1.26469282800573,-8.10235283801081,2.17005725520049));
#8735=CARTESIAN_POINT('Ctrl Pts',(1.3911621108063,-8.96588232345381,-0.576701529052951));
#8736=CARTESIAN_POINT('Ctrl Pts',(1.51763139360688,-7.13601528805713,-2.7997267301126));
#8737=CARTESIAN_POINT('Ctrl Pts',(1.64410067640745,-4.27451231466393,-2.48026509630649));
#8738=CARTESIAN_POINT('Ctrl Pts',(1.77056995920802,-2.97996136626914,0.0915870049917526));
#8739=CARTESIAN_POINT('Ctrl Pts',(1.8970392420086,-4.42797832080538,2.58026432327149));
#8740=CARTESIAN_POINT('Ctrl Pts',(2.02350852480917,-7.30358342959944,2.725745728157));
#8741=CARTESIAN_POINT('Ctrl Pts',(2.14997780760974,-8.99537493549262,0.395914211910863));
#8742=CARTESIAN_POINT('Ctrl Pts',(2.27644709041031,-7.9669975211319,-2.29345572403429));
#8743=CARTESIAN_POINT('Ctrl Pts',(2.40291637321089,-5.15234464286247,-2.90008608592962));
#8744=CARTESIAN_POINT('Ctrl Pts',(2.52938565601146,-3.10746698267462,-0.873081638157841));
#8745=CARTESIAN_POINT('Ctrl Pts',(2.65585493881204,-3.68936495023107,1.94678822513078));
#8746=CARTESIAN_POINT('Ctrl Pts',(2.7823242216126,-6.36960360330106,2.99873506265578));
#8747=CARTESIAN_POINT('Ctrl Pts',(2.90879350441318,-8.71419675286107,1.32746177559001));
#8748=CARTESIAN_POINT('Ctrl Pts',(3.03526278721375,-8.59396555469508,-1.5493099986334));
#8749=CARTESIAN_POINT('Ctrl Pts',(3.16173207001433,-6.1180947250836,-3.01911782098221));
#8750=CARTESIAN_POINT('Ctrl Pts',(3.2882013528149,-3.53497936495718,-1.74719548025824));
#8751=CARTESIAN_POINT('Ctrl Pts',(3.41467063561547,-3.19040579929669,1.11139516108156));
#8752=CARTESIAN_POINT('Ctrl Pts',(3.54113991841605,-5.39728918769256,2.96070235836602));
#8753=CARTESIAN_POINT('Ctrl Pts',(3.66760920121662,-8.15150809295624,2.12132781612021));
#8754=CARTESIAN_POINT('Ctrl Pts',(3.79407848401719,-8.95189313670652,-0.644473185577155));
#8755=CARTESIAN_POINT('Ctrl Pts',(3.92054776681777,-7.07159629755764,-2.82501330133343));
#8756=CARTESIAN_POINT('Ctrl Pts',(4.04701704961834,-4.21815827485875,-2.44009402361868));
#8757=CARTESIAN_POINT('Ctrl Pts',(4.17348633241891,-2.98285160370029,0.160730620181111));
#8758=CARTESIAN_POINT('Ctrl Pts',(4.29995561521949,-4.48748661387422,2.61559210015096));
#8759=CARTESIAN_POINT('Ctrl Pts',(4.42642489802005,-7.36566973169923,2.69517438424447));
#8760=CARTESIAN_POINT('Ctrl Pts',(4.55289418082063,-9.00365683350444,0.327206974422883));
#8761=CARTESIAN_POINT('Ctrl Pts',(4.67936346362121,-7.9139542516838,-2.33790459600758));
#8762=CARTESIAN_POINT('Ctrl Pts',(4.80583274642177,-5.08614590191431,-2.87991136408426));
#8763=CARTESIAN_POINT('Ctrl Pts',(4.93230202922235,-3.08822942523902,-0.806604548416513));
#8764=CARTESIAN_POINT('Ctrl Pts',(5.05877131202292,-3.73455861247221,1.99919836365645));
#8765=CARTESIAN_POINT('Ctrl Pts',(5.1852405948235,-6.43818709990916,2.98948337393659));
#8766=CARTESIAN_POINT('Ctrl Pts',(5.31170987762407,-8.74388782855944,1.26494994440632));
#8767=CARTESIAN_POINT('Ctrl Pts',(5.43817916042464,-8.55780106687306,-1.60831355147971));
#8768=CARTESIAN_POINT('Ctrl Pts',(5.56464844322523,-6.04891647253973,-3.02103061160996));
#8769=CARTESIAN_POINT('Ctrl Pts',(5.69111772602578,-3.49560970719883,-1.69028046160792));
#8770=CARTESIAN_POINT('Ctrl Pts',(5.81758700882637,-3.21659722516281,1.17545215581023));
#8771=CARTESIAN_POINT('Ctrl Pts',(5.94405629162693,-5.4652566627727,2.97372970205115));
#8772=CARTESIAN_POINT('Ctrl Pts',(6.07052557442751,-8.19952879357467,2.0714950793584));
#8773=CARTESIAN_POINT('Ctrl Pts',(6.19699485722808,-8.9363583629794,-0.711911751364896));
#8774=CARTESIAN_POINT('Ctrl Pts',(6.32346414002865,-7.00661353387476,-2.84881518722965));
#8775=CARTESIAN_POINT('Ctrl Pts',(6.44993342282923,-4.16273985984979,-2.39864419099309));
#8776=CARTESIAN_POINT('Ctrl Pts',(6.5764027056298,-2.98732427149032,0.22979062735577));
#8777=CARTESIAN_POINT('Ctrl Pts',(6.70287198843037,-4.54778863223406,2.64954730489951));
#8778=CARTESIAN_POINT('Ctrl Pts',(6.82934127123096,-7.42703945423727,2.66318928610364));
#8779=CARTESIAN_POINT('Ctrl Pts',(6.95581055403151,-9.01036300717914,0.25832797484807));
#8780=CARTESIAN_POINT('Ctrl Pts',(7.0822798368321,-7.85990684631327,-2.38112689720535));
#8781=CARTESIAN_POINT('Ctrl Pts',(7.20874911963266,-5.02042660634255,-2.85822580353484));
#8782=CARTESIAN_POINT('Ctrl Pts',(7.33521840243325,-3.07051943955244,-0.739704281189414));
#8783=CARTESIAN_POINT('Ctrl Pts',(7.4616876852338,-3.78094078104177,2.05055966999733));
#8784=CARTESIAN_POINT('Ctrl Pts',(7.58815696803439,-6.50654071121665,2.97866333871112));
#8785=CARTESIAN_POINT('Ctrl Pts',(7.71462625083495,-8.77213940010801,1.20177448985872));
#8786=CARTESIAN_POINT('Ctrl Pts',(7.84109553363553,-8.52029469802955,-1.66647334565703));
#8787=CARTESIAN_POINT('Ctrl Pts',(7.96756481643611,-5.9797125579978,-3.02135850191909));
#8788=CARTESIAN_POINT('Ctrl Pts',(8.09403409923667,-3.4575539082881,-1.63247868341485));
#8789=CARTESIAN_POINT('Ctrl Pts',(8.22050338203725,-3.24424888831968,1.23889248172823));
#8790=CARTESIAN_POINT('Ctrl Pts',(8.34697266483782,-5.5335046738129,2.98519695992403));
#8791=CARTESIAN_POINT('Ctrl Pts',(8.47344194763839,-8.24639557638579,2.02057558976858));
#8792=CARTESIAN_POINT('Ctrl Pts',(8.59991123043898,-8.91928310048972,-0.77897683272588));
#8793=CARTESIAN_POINT('Ctrl Pts',(8.72638051323954,-6.94110269497493,-2.87112251928));
#8794=CARTESIAN_POINT('Ctrl Pts',(8.85284979604013,-4.10828528051702,-2.35593597756347));
#8795=CARTESIAN_POINT('Ctrl Pts',(8.97931907884068,-2.99337751913424,0.298730085189438));
#8796=CARTESIAN_POINT('Ctrl Pts',(9.10578836164126,-4.60885239449141,2.68211248963539));
#8797=CARTESIAN_POINT('Ctrl Pts',(9.23225764444184,-7.48766074739694,2.6298070334431));
#8798=CARTESIAN_POINT('Ctrl Pts',(9.3587269272424,-9.01548944052047,0.189313422437645));
#8799=CARTESIAN_POINT('Ctrl Pts',(9.48519621004299,-7.80488452630467,-2.42309995159429));
#8800=CARTESIAN_POINT('Ctrl Pts',(9.61166549284354,-4.95521961969974,-2.83504085634446));
#8801=CARTESIAN_POINT('Ctrl Pts',(9.73813477564413,-3.05434938326512,-0.672415750957662));
#8802=CARTESIAN_POINT('Ctrl Pts',(9.86460405844471,-3.82848126493051,2.10084482849876));
#8803=CARTESIAN_POINT('Ctrl Pts',(9.99107334124527,-6.57463978426254,2.96628135292037));
#8804=CARTESIAN_POINT('Ctrl Pts',(10.1175426240459,-8.79891519692859,1.13796717239844));
#8805=CARTESIAN_POINT('Ctrl Pts',(10.2440119068464,-8.4815071817026,-1.72375621929785));
#8806=CARTESIAN_POINT('Ctrl Pts',(10.370481189647,-5.91044069571119,-3.02010639410425));
#8807=CARTESIAN_POINT('Ctrl Pts',(10.4969504724476,-3.42098237960844,-1.57381075447018));
#8808=CARTESIAN_POINT('Ctrl Pts',(10.6234197552481,-3.27305825140319,1.30166424671849));
#8809=CARTESIAN_POINT('Ctrl Pts',(10.7498890380487,-5.60254915406858,2.99513384905324));
#8810=CARTESIAN_POINT('Ctrl Pts',(10.8763583208493,-8.29102426622762,1.96852667642011));
#8811=CARTESIAN_POINT('Ctrl Pts',(11.0028276036498,-8.90273551252011,-0.8454915895703));
#8812=CARTESIAN_POINT('Ctrl Pts',(11.1292968864504,-6.870879053568,-2.89227340548826));
#8813=CARTESIAN_POINT('Ctrl Pts',(11.2136097416508,-5.00047342783812,-2.50459204726911));
#8814=CARTESIAN_POINT('Ctrl Pts',(11.255766169251,-4.35188695942431,-1.9589087282169));
#8815=CARTESIAN_POINT('Ctrl Pts',(-0.0852553897503347,-5.37643325356376,
-2.33034688916694));
#8816=CARTESIAN_POINT('Ctrl Pts',(-0.0430989621501437,-4.60486516708142,
-2.12388655333521));
#8817=CARTESIAN_POINT('Ctrl Pts',(0.0412138930502385,-3.29587975786923,
-0.888378950851187));
#8818=CARTESIAN_POINT('Ctrl Pts',(0.167683175850811,-3.78020116694325,1.7858106391383));
#8819=CARTESIAN_POINT('Ctrl Pts',(0.294152458651385,-6.28399216264951,2.83214082296819));
#8820=CARTESIAN_POINT('Ctrl Pts',(0.420621741451957,-8.52804525286687,1.30958596056379));
#8821=CARTESIAN_POINT('Ctrl Pts',(0.547091024252532,-8.47727684407722,-1.40380876252277));
#8822=CARTESIAN_POINT('Ctrl Pts',(0.673560307053103,-6.17633856500803,-2.84155174293356));
#8823=CARTESIAN_POINT('Ctrl Pts',(0.800029589853677,-3.71552323896728,-1.69924497029643));
#8824=CARTESIAN_POINT('Ctrl Pts',(0.926498872654249,-3.32915782945394,0.986409013851733));
#8825=CARTESIAN_POINT('Ctrl Pts',(1.05296815545482,-5.36831643648831,2.77616539417007));
#8826=CARTESIAN_POINT('Ctrl Pts',(1.17943743825539,-7.98108430842242,2.04488337967265));
#8827=CARTESIAN_POINT('Ctrl Pts',(1.30590672105597,-8.79480343422335,-0.543436063249505));
#8828=CARTESIAN_POINT('Ctrl Pts',(1.43237600385654,-7.07048732287362,-2.63823207627928));
#8829=CARTESIAN_POINT('Ctrl Pts',(1.55884528665711,-4.37404239859673,-2.33719772161069));
#8830=CARTESIAN_POINT('Ctrl Pts',(1.68531456945769,-3.1541641155846,0.0863040566569423));
#8831=CARTESIAN_POINT('Ctrl Pts',(1.81178385225826,-4.51865613381102,2.43142876399945));
#8832=CARTESIAN_POINT('Ctrl Pts',(1.93825313505883,-7.22838975000144,2.56851846805628));
#8833=CARTESIAN_POINT('Ctrl Pts',(2.06472241785941,-8.82259484481252,0.373076972864443));
#8834=CARTESIAN_POINT('Ctrl Pts',(2.19119170065998,-7.85353659641036,-2.16116394203596));
#8835=CARTESIAN_POINT('Ctrl Pts',(2.31766098346055,-5.20123934640569,-2.73280247446258));
#8836=CARTESIAN_POINT('Ctrl Pts',(2.44413026626113,-3.27431491583545,-0.822720288456811));
#8837=CARTESIAN_POINT('Ctrl Pts',(2.5705995490617,-3.82264767510706,1.83449301891556));
#8838=CARTESIAN_POINT('Ctrl Pts',(2.69706883186227,-6.34828402045441,2.82576115214061));
#8839=CARTESIAN_POINT('Ctrl Pts',(2.82353811466284,-8.55763566412181,1.25089073827407));
#8840=CARTESIAN_POINT('Ctrl Pts',(2.95000739746342,-8.44433967699588,-1.45994224741015));
#8841=CARTESIAN_POINT('Ctrl Pts',(3.07647668026399,-6.11128275070704,-2.84496818625629));
#8842=CARTESIAN_POINT('Ctrl Pts',(3.20294596306457,-3.67716740419206,-1.6464132409673));
#8843=CARTESIAN_POINT('Ctrl Pts',(3.32941524586514,-3.35246963144664,1.04728734124313));
#8844=CARTESIAN_POINT('Ctrl Pts',(3.45588452866571,-5.43205492855872,2.78992226139257));
#8845=CARTESIAN_POINT('Ctrl Pts',(3.58235381146628,-8.02740417561515,1.99896476631015));
#8846=CARTESIAN_POINT('Ctrl Pts',(3.70882309426686,-8.78162117582619,-0.607298495315348));
#8847=CARTESIAN_POINT('Ctrl Pts',(3.83529237706743,-7.009784167373,-2.66206006012371));
#8848=CARTESIAN_POINT('Ctrl Pts',(3.96176165986801,-4.32093898895219,-2.29934380845422));
#8849=CARTESIAN_POINT('Ctrl Pts',(4.08823094266858,-3.15688763749726,0.151459309668061));
#8850=CARTESIAN_POINT('Ctrl Pts',(4.21470022546915,-4.57473185216246,2.46471875374903));
#8851=CARTESIAN_POINT('Ctrl Pts',(4.34116950826972,-7.28689477191502,2.53971054931996));
#8852=CARTESIAN_POINT('Ctrl Pts',(4.46763879107029,-8.83039902396766,0.308332926288854));
#8853=CARTESIAN_POINT('Ctrl Pts',(4.59410807387087,-7.80355298430152,-2.20304890121183));
#8854=CARTESIAN_POINT('Ctrl Pts',(4.72057735667144,-5.13885910054086,-2.713791476807));
#8855=CARTESIAN_POINT('Ctrl Pts',(4.84704663947202,-3.2561870247988,-0.760077749595094));
#8856=CARTESIAN_POINT('Ctrl Pts',(4.97351592227259,-3.86523446334132,1.8838800205445));
#8857=CARTESIAN_POINT('Ctrl Pts',(5.09998520507316,-6.41291146380764,2.81704312202853));
#8858=CARTESIAN_POINT('Ctrl Pts',(5.22645448787374,-8.58561409053185,1.19198473276934));
#8859=CARTESIAN_POINT('Ctrl Pts',(5.35292377067431,-8.41026123970837,-1.51554234011181));
#8860=CARTESIAN_POINT('Ctrl Pts',(5.47939305347488,-6.0460948583034,-2.84677064273715));
#8861=CARTESIAN_POINT('Ctrl Pts',(5.60586233627545,-3.64006867851535,-1.59278121102298));
#8862=CARTESIAN_POINT('Ctrl Pts',(5.73233161907603,-3.37715027584678,1.10764938171857));
#8863=CARTESIAN_POINT('Ctrl Pts',(5.85880090187659,-5.49610188391745,2.80219815803961));
#8864=CARTESIAN_POINT('Ctrl Pts',(5.98527018467719,-8.07265493217446,1.95200649600478));
#8865=CARTESIAN_POINT('Ctrl Pts',(6.11173946747773,-8.76698248344817,-0.67084705008174));
#8866=CARTESIAN_POINT('Ctrl Pts',(6.23820875027832,-6.94854975841818,-2.68448899869544));
#8867=CARTESIAN_POINT('Ctrl Pts',(6.36467803307889,-4.26871723512147,-2.26028489716367));
#8868=CARTESIAN_POINT('Ctrl Pts',(6.49114731587947,-3.1611023115593,0.216535777366369));
#8869=CARTESIAN_POINT('Ctrl Pts',(6.61761659868004,-4.63155551191118,2.49671534447367));
#8870=CARTESIAN_POINT('Ctrl Pts',(6.74408588148062,-7.34472454821811,2.50957042493907));
#8871=CARTESIAN_POINT('Ctrl Pts',(6.87055516428118,-8.83671837017649,0.243427025257224));
#8872=CARTESIAN_POINT('Ctrl Pts',(6.99702444708176,-7.7526231571314,-2.24377804102541));
#8873=CARTESIAN_POINT('Ctrl Pts',(7.12349372988232,-5.07693064454441,-2.69335678908615));
#8874=CARTESIAN_POINT('Ctrl Pts',(7.2499630126829,-3.23949859167201,-0.697036443094767));
#8875=CARTESIAN_POINT('Ctrl Pts',(7.37643229548348,-3.90894120213532,1.93227868903264));
#8876=CARTESIAN_POINT('Ctrl Pts',(7.50290157828405,-6.4773222821712,2.80684721123077));
#8877=CARTESIAN_POINT('Ctrl Pts',(7.62937086108462,-8.61223604669034,1.13245338321713));
#8878=CARTESIAN_POINT('Ctrl Pts',(7.7558401438852,-8.37491832417184,-1.57034734407812));
#8879=CARTESIAN_POINT('Ctrl Pts',(7.88230942668576,-5.98088278414455,-2.84707961958182));
#8880=CARTESIAN_POINT('Ctrl Pts',(8.00877870948635,-3.604208025297,-1.5383135718585));
#8881=CARTESIAN_POINT('Ctrl Pts',(8.13524799228691,-3.40320692770437,1.16743032425354));
#8882=CARTESIAN_POINT('Ctrl Pts',(8.26171727508749,-5.56041319327916,2.81300395819925));
#8883=CARTESIAN_POINT('Ctrl Pts',(8.38818655788806,-8.11681833154999,1.904024159265));
#8884=CARTESIAN_POINT('Ctrl Pts',(8.51465584068864,-8.7508921612297,-0.734043663859012));
#8885=CARTESIAN_POINT('Ctrl Pts',(8.6411251234892,-6.8868177348351,-2.70550959271215));
#8886=CARTESIAN_POINT('Ctrl Pts',(8.7675944062898,-4.21740372071637,-2.22004019135766));
#8887=CARTESIAN_POINT('Ctrl Pts',(8.89406368909034,-3.1668063940071,0.281498649285935));
#8888=CARTESIAN_POINT('Ctrl Pts',(9.02053297189093,-4.68909697642373,2.52740209472543));
#8889=CARTESIAN_POINT('Ctrl Pts',(9.1470022546915,-7.40184906626454,2.47811373711298));
#8890=CARTESIAN_POINT('Ctrl Pts',(9.27347153749207,-8.8415490990946,0.178393390388182));
#8891=CARTESIAN_POINT('Ctrl Pts',(9.39994082029265,-7.70077465063371,-2.28332999344895));
#8892=CARTESIAN_POINT('Ctrl Pts',(9.52641010309321,-5.01548494632383,-2.67150920278189));
#8893=CARTESIAN_POINT('Ctrl Pts',(9.6528793858938,-3.22426126128772,-0.633629269489662));
#8894=CARTESIAN_POINT('Ctrl Pts',(9.77934866869436,-3.95373944196641,1.97966328435488));
#8895=CARTESIAN_POINT('Ctrl Pts',(9.90581795149494,-6.54149324462344,2.79517944675582));
#8896=CARTESIAN_POINT('Ctrl Pts',(10.0322872342955,-8.63746735418908,1.07232661805306));
#8897=CARTESIAN_POINT('Ctrl Pts',(10.1587565170961,-8.33836816067471,-1.62432601029408));
#8898=CARTESIAN_POINT('Ctrl Pts',(10.2852257998966,-5.91560668162263,-2.84589973621517));
#8899=CARTESIAN_POINT('Ctrl Pts',(10.4116950826972,-3.56974602620135,-1.48302974350269));
#8900=CARTESIAN_POINT('Ctrl Pts',(10.5381643654978,-3.43035450070375,1.22658126998721));
#8901=CARTESIAN_POINT('Ctrl Pts',(10.6646336482984,-5.62547502968677,2.82236766479144));
#8902=CARTESIAN_POINT('Ctrl Pts',(10.791102931099,-8.15887273628766,1.85497754651723));
#8903=CARTESIAN_POINT('Ctrl Pts',(10.9175722138995,-8.73529907605575,-0.796721697098993));
#8904=CARTESIAN_POINT('Ctrl Pts',(11.0440414967001,-6.82064475399369,-2.72544044733314));
#8905=CARTESIAN_POINT('Ctrl Pts',(11.1283543519005,-5.05812841110215,-2.36012143829251));
#8906=CARTESIAN_POINT('Ctrl Pts',(11.1705107795007,-4.44695389653044,-1.84591438360752));
#8907=CARTESIAN_POINT('Ctrl Pts',(-0.170510779500669,-5.41460377569604,
-2.18769887591546));
#8908=CARTESIAN_POINT('Ctrl Pts',(-0.128354351900478,-4.69026584843874,
-1.9938766399557));
#8909=CARTESIAN_POINT('Ctrl Pts',(-0.0440414967000964,-3.46140763782832,
-0.833998423667675));
#8910=CARTESIAN_POINT('Ctrl Pts',(0.0824277861004769,-3.91608217883272,
1.6764954376545));
#8911=CARTESIAN_POINT('Ctrl Pts',(0.208897068901049,-6.26660809078911,2.6587763923236));
#8912=CARTESIAN_POINT('Ctrl Pts',(0.335366351701623,-8.3732954881826,1.22942200028608));
#8913=CARTESIAN_POINT('Ctrl Pts',(0.461835634502196,-8.32563477665615,-1.31787712209198));
#8914=CARTESIAN_POINT('Ctrl Pts',(0.58830491730277,-6.16554431541587,-2.66761123966984));
#8915=CARTESIAN_POINT('Ctrl Pts',(0.714774200103341,-3.85536339443742,-1.59522873126902));
#8916=CARTESIAN_POINT('Ctrl Pts',(0.841243482903916,-3.49264865183227,0.926027751845885));
#8917=CARTESIAN_POINT('Ctrl Pts',(0.967712765704488,-5.40698381504787,2.60622739919738));
#8918=CARTESIAN_POINT('Ctrl Pts',(1.09418204850506,-7.85981577883405,1.91970950414481));
#8919=CARTESIAN_POINT('Ctrl Pts',(1.22065133130563,-8.62372454499285,-0.510170597446061));
#8920=CARTESIAN_POINT('Ctrl Pts',(1.34712061410621,-7.00495935769013,-2.47673742244596));
#8921=CARTESIAN_POINT('Ctrl Pts',(1.47358989690678,-4.47357248252952,-2.19413034691488));
#8922=CARTESIAN_POINT('Ctrl Pts',(1.60005917970735,-3.32836686490007,0.0810211083221311));
#8923=CARTESIAN_POINT('Ctrl Pts',(1.72652846250793,-4.60933394681663,2.28259320472741));
#8924=CARTESIAN_POINT('Ctrl Pts',(1.8529977453085,-7.15319607040347,2.41129120795556));
#8925=CARTESIAN_POINT('Ctrl Pts',(1.97946702810907,-8.64981475413239,0.350239733818021));
#8926=CARTESIAN_POINT('Ctrl Pts',(2.10593631090965,-7.74007567168883,-2.02887216003762));
#8927=CARTESIAN_POINT('Ctrl Pts',(2.23240559371022,-5.2501340499489,-2.56551886299555));
#8928=CARTESIAN_POINT('Ctrl Pts',(2.35887487651079,-3.44116284899628,-0.772358938755779));
#8929=CARTESIAN_POINT('Ctrl Pts',(2.48534415931136,-3.95593039998305,1.72219781270033));
#8930=CARTESIAN_POINT('Ctrl Pts',(2.61181344211194,-6.32696443760774,2.65278724162544));
#8931=CARTESIAN_POINT('Ctrl Pts',(2.73828272491251,-8.40107457538256,1.17431970095814));
#8932=CARTESIAN_POINT('Ctrl Pts',(2.86475200771309,-8.29471379929668,-1.37057449618689));
#8933=CARTESIAN_POINT('Ctrl Pts',(2.99122129051366,-6.10447077633046,-2.67081855153036));
#8934=CARTESIAN_POINT('Ctrl Pts',(3.11769057331424,-3.81935544342696,-1.54563100167637));
#8935=CARTESIAN_POINT('Ctrl Pts',(3.2441598561148,-3.51453346359658,0.983179521404702));
#8936=CARTESIAN_POINT('Ctrl Pts',(3.37062913891538,-5.4668206694249,2.61914216441911));
#8937=CARTESIAN_POINT('Ctrl Pts',(3.49709842171595,-7.90330025827405,1.87660171650009));
#8938=CARTESIAN_POINT('Ctrl Pts',(3.62356770451653,-8.61134921494586,-0.570123805053538));
#8939=CARTESIAN_POINT('Ctrl Pts',(3.75003698731709,-6.94797203718836,-2.49910681891398));
#8940=CARTESIAN_POINT('Ctrl Pts',(3.87650627011767,-4.42371970304562,-2.15859359328975));
#8941=CARTESIAN_POINT('Ctrl Pts',(4.00297555291824,-3.33092367129424,0.142187999155009));
#8942=CARTESIAN_POINT('Ctrl Pts',(4.12944483571882,-4.66197709045071,2.31384540734709));
#8943=CARTESIAN_POINT('Ctrl Pts',(4.25591411851939,-7.2081198121308,2.38424671439544));
#8944=CARTESIAN_POINT('Ctrl Pts',(4.38238340131996,-8.65714121443088,0.289458878154826));
#8945=CARTESIAN_POINT('Ctrl Pts',(4.50885268412053,-7.69315171691924,-2.06819320641608));
#8946=CARTESIAN_POINT('Ctrl Pts',(4.63532196692111,-5.19157229916742,-2.54767158952975));
#8947=CARTESIAN_POINT('Ctrl Pts',(4.76179124972168,-3.42414462435858,-0.71355095077367));
#8948=CARTESIAN_POINT('Ctrl Pts',(4.88826053252226,-3.99591031421044,1.76856167743254));
#8949=CARTESIAN_POINT('Ctrl Pts',(5.01472981532283,-6.3876358277061,2.64460287012047));
#8950=CARTESIAN_POINT('Ctrl Pts',(5.1411990981234,-8.42734035250428,1.11901952113236));
#8951=CARTESIAN_POINT('Ctrl Pts',(5.26766838092397,-8.26272141254368,-1.4227711287439));
#8952=CARTESIAN_POINT('Ctrl Pts',(5.39413766372455,-6.04327324406706,-2.67251067386434));
#8953=CARTESIAN_POINT('Ctrl Pts',(5.52060694652512,-3.78452764983187,-1.49528196043805));
#8954=CARTESIAN_POINT('Ctrl Pts',(5.64707622932569,-3.53770332653075,1.03984660762691));
#8955=CARTESIAN_POINT('Ctrl Pts',(5.77354551212626,-5.52694710506219,2.63066661402806));
#8956=CARTESIAN_POINT('Ctrl Pts',(5.90001479492685,-7.94578107077427,1.83251791265116));
#8957=CARTESIAN_POINT('Ctrl Pts',(6.0264840777274,-8.59760660391693,-0.629782348798582));
#8958=CARTESIAN_POINT('Ctrl Pts',(6.15295336052799,-6.8904859829616,-2.52016281016122));
#8959=CARTESIAN_POINT('Ctrl Pts',(6.27942264332856,-4.37469461039316,-2.12192560333425));
#8960=CARTESIAN_POINT('Ctrl Pts',(6.40589192612913,-3.33488035162828,0.203280927376966));
#8961=CARTESIAN_POINT('Ctrl Pts',(6.53236120892971,-4.71532239158831,2.34388338404782));
#8962=CARTESIAN_POINT('Ctrl Pts',(6.65883049173027,-7.26240964219896,2.3559515637745));
#8963=CARTESIAN_POINT('Ctrl Pts',(6.78529977453086,-8.66307373317385,0.228526075666379));
#8964=CARTESIAN_POINT('Ctrl Pts',(6.91176905733142,-7.64533946794951,-2.10642918484546));
#8965=CARTESIAN_POINT('Ctrl Pts',(7.038238340132,-5.13343468274627,-2.52848777463746));
#8966=CARTESIAN_POINT('Ctrl Pts',(7.16470762293256,-3.40847774379157,-0.654368605000115));
#8967=CARTESIAN_POINT('Ctrl Pts',(7.29117690573314,-4.03694162322887,1.81399770806795));
#8968=CARTESIAN_POINT('Ctrl Pts',(7.41764618853371,-6.44810385312578,2.63503108375044));
#8969=CARTESIAN_POINT('Ctrl Pts',(7.54411547133429,-8.45233269327263,1.06313227657554));
#8970=CARTESIAN_POINT('Ctrl Pts',(7.67058475413486,-8.22954195031416,-1.47422134249921));
#8971=CARTESIAN_POINT('Ctrl Pts',(7.79705403693543,-5.98205301029128,-2.67280073724457));
#8972=CARTESIAN_POINT('Ctrl Pts',(7.92352331973601,-3.75086214230591,-1.44414846030215));
#8973=CARTESIAN_POINT('Ctrl Pts',(8.04999260253658,-3.56216496708905,1.09596816677885));
#8974=CARTESIAN_POINT('Ctrl Pts',(8.17646188533715,-5.58732171274542,2.64081095647447));
#8975=CARTESIAN_POINT('Ctrl Pts',(8.30293116813773,-7.9872410867142,1.78747272876143));
#8976=CARTESIAN_POINT('Ctrl Pts',(8.4294004509383,-8.58250122196968,-0.689110494992141));
#8977=CARTESIAN_POINT('Ctrl Pts',(8.55586973373887,-6.83253277469527,-2.53989666614431));
#8978=CARTESIAN_POINT('Ctrl Pts',(8.68233901653945,-4.32652216091571,-2.08414440515185));
#8979=CARTESIAN_POINT('Ctrl Pts',(8.80880829934001,-3.34023526887996,0.264267213382427));
#8980=CARTESIAN_POINT('Ctrl Pts',(8.9352775821406,-4.76934155835606,2.37269169981547));
#8981=CARTESIAN_POINT('Ctrl Pts',(9.06174686494116,-7.31603738513214,2.32642044078287));
#8982=CARTESIAN_POINT('Ctrl Pts',(9.18821614774174,-8.66760875766876,0.16747335833872));
#8983=CARTESIAN_POINT('Ctrl Pts',(9.31468543054231,-7.59666477496275,-2.1435600353036));
#8984=CARTESIAN_POINT('Ctrl Pts',(9.44115471334288,-5.07575027294792,-2.50797754921931));
#8985=CARTESIAN_POINT('Ctrl Pts',(9.56762399614347,-3.39417313931032,-0.594842788021662));
#8986=CARTESIAN_POINT('Ctrl Pts',(9.69409327894402,-4.07899761900233,1.85848174021101));
#8987=CARTESIAN_POINT('Ctrl Pts',(9.82056256174462,-6.50834670498434,2.62407754059128));
#8988=CARTESIAN_POINT('Ctrl Pts',(9.94703184454517,-8.47601951144958,1.00668606370768));
#8989=CARTESIAN_POINT('Ctrl Pts',(10.0735011273458,-8.19522913964682,-1.52489580129031));
#8990=CARTESIAN_POINT('Ctrl Pts',(10.1999704101463,-5.92077266753408,-2.67169307832608));
#8991=CARTESIAN_POINT('Ctrl Pts',(10.3264396929469,-3.71850967279424,-1.39224873253521));
#8992=CARTESIAN_POINT('Ctrl Pts',(10.4529089757475,-3.58765075000433,1.15149829325592));
#8993=CARTESIAN_POINT('Ctrl Pts',(10.579378258548,-5.64840090530495,2.64960148052965));
#8994=CARTESIAN_POINT('Ctrl Pts',(10.7058475413486,-8.02672120634771,1.74142841661435));
#8995=CARTESIAN_POINT('Ctrl Pts',(10.8323168241492,-8.56786263959136,-0.747951804627684));
#8996=CARTESIAN_POINT('Ctrl Pts',(10.9587861069498,-6.7704104544194,-2.55860748917802));
#8997=CARTESIAN_POINT('Ctrl Pts',(11.0430989621501,-5.11578339436617,-2.21565082931592));
#8998=CARTESIAN_POINT('Ctrl Pts',(11.0852553897503,-4.54202083363656,-1.73292003899813));
#8999=CARTESIAN_POINT('Ctrl Pts',(-0.255766169251004,-5.45277429782831,
-2.04505086266398));
#9000=CARTESIAN_POINT('Ctrl Pts',(-0.213609741650813,-4.77566652979606,
-1.8638667265762));
#9001=CARTESIAN_POINT('Ctrl Pts',(-0.129296886450431,-3.62693551778741,
-0.779617896484163));
#9002=CARTESIAN_POINT('Ctrl Pts',(-0.00282760364985816,-4.0519631907222,
1.5671802361707));
#9003=CARTESIAN_POINT('Ctrl Pts',(0.123641679150715,-6.24922401892871,2.48541196167901));
#9004=CARTESIAN_POINT('Ctrl Pts',(0.250110961951288,-8.21854572349833,1.14925804000838));
#9005=CARTESIAN_POINT('Ctrl Pts',(0.376580244751862,-8.1739927092351,-1.2319454816612));
#9006=CARTESIAN_POINT('Ctrl Pts',(0.503049527552435,-6.15475006582368,-2.49367073640612));
#9007=CARTESIAN_POINT('Ctrl Pts',(0.629518810353007,-3.99520354990758,-1.49121249224162));
#9008=CARTESIAN_POINT('Ctrl Pts',(0.755988093153581,-3.65613947421059,0.865646489840036));
#9009=CARTESIAN_POINT('Ctrl Pts',(0.882457375954153,-5.44565119360746,2.43628940422469));
#9010=CARTESIAN_POINT('Ctrl Pts',(1.00892665875473,-7.73854724924566,1.79453562861697));
#9011=CARTESIAN_POINT('Ctrl Pts',(1.1353959415553,-8.45264565576239,-0.476905131642614));
#9012=CARTESIAN_POINT('Ctrl Pts',(1.26186522435587,-6.93943139250662,-2.31524276861265));
#9013=CARTESIAN_POINT('Ctrl Pts',(1.38833450715645,-4.57310256646231,-2.05106297221908));
#9014=CARTESIAN_POINT('Ctrl Pts',(1.51480378995702,-3.50256961421554,0.0757381599873213));
#9015=CARTESIAN_POINT('Ctrl Pts',(1.64127307275759,-4.70001175982226,2.13375764545536));
#9016=CARTESIAN_POINT('Ctrl Pts',(1.76774235555817,-7.07800239080548,2.25406394785483));
#9017=CARTESIAN_POINT('Ctrl Pts',(1.89421163835874,-8.4770346634523,0.327402494771599));
#9018=CARTESIAN_POINT('Ctrl Pts',(2.02068092115931,-7.62661474696728,-1.89658037803929));
#9019=CARTESIAN_POINT('Ctrl Pts',(2.14715020395988,-5.29902875349213,-2.39823525152852));
#9020=CARTESIAN_POINT('Ctrl Pts',(2.27361948676046,-3.60801078215711,-0.721997589054746));
#9021=CARTESIAN_POINT('Ctrl Pts',(2.40008876956103,-4.08921312485905,1.6099026064851));
#9022=CARTESIAN_POINT('Ctrl Pts',(2.5265580523616,-6.30564485476107,2.47981333111027));
#9023=CARTESIAN_POINT('Ctrl Pts',(2.65302733516218,-8.24451348664331,1.0977486636422));
#9024=CARTESIAN_POINT('Ctrl Pts',(2.77949661796275,-8.14508792159745,-1.28120674496364));
#9025=CARTESIAN_POINT('Ctrl Pts',(2.90596590076332,-6.09765880195391,-2.49666891680443));
#9026=CARTESIAN_POINT('Ctrl Pts',(3.0324351835639,-3.96154348266185,-1.44484876238543));
#9027=CARTESIAN_POINT('Ctrl Pts',(3.15890446636447,-3.67659729574652,0.919071701566275));
#9028=CARTESIAN_POINT('Ctrl Pts',(3.28537374916505,-5.50158641029108,2.44836206744565));
#9029=CARTESIAN_POINT('Ctrl Pts',(3.41184303196561,-7.77919634093294,1.75423866669003));
#9030=CARTESIAN_POINT('Ctrl Pts',(3.53831231476619,-8.44107725406553,-0.532949114791734));
#9031=CARTESIAN_POINT('Ctrl Pts',(3.66478159756675,-6.88615990700371,-2.33615357770425));
#9032=CARTESIAN_POINT('Ctrl Pts',(3.79125088036734,-4.52650041713906,-2.01784337812529));
#9033=CARTESIAN_POINT('Ctrl Pts',(3.91772016316791,-3.50495970509121,0.132916688641959));
#9034=CARTESIAN_POINT('Ctrl Pts',(4.04418944596848,-4.74922232873896,2.16297206094515));
#9035=CARTESIAN_POINT('Ctrl Pts',(4.17065872876906,-7.12934485234659,2.22878287947092));
#9036=CARTESIAN_POINT('Ctrl Pts',(4.29712801156963,-8.48388340489409,0.270584830020798));
#9037=CARTESIAN_POINT('Ctrl Pts',(4.4235972943702,-7.58275044953696,-1.93333751162033));
#9038=CARTESIAN_POINT('Ctrl Pts',(4.55006657717077,-5.24428549779397,-2.38155170225249));
#9039=CARTESIAN_POINT('Ctrl Pts',(4.67653585997135,-3.59210222391837,-0.66702415195225));
#9040=CARTESIAN_POINT('Ctrl Pts',(4.80300514277192,-4.12658616507955,1.65324333432059));
#9041=CARTESIAN_POINT('Ctrl Pts',(4.92947442557249,-6.36236019160457,2.47216261821241));
#9042=CARTESIAN_POINT('Ctrl Pts',(5.05594370837307,-8.26906661447669,1.04605430949538));
#9043=CARTESIAN_POINT('Ctrl Pts',(5.18241299117363,-8.11518158537901,-1.32999991737599));
#9044=CARTESIAN_POINT('Ctrl Pts',(5.30888227397421,-6.04045162983072,-2.49825070499153));
#9045=CARTESIAN_POINT('Ctrl Pts',(5.43535155677479,-3.9289866211484,-1.39778270985311));
#9046=CARTESIAN_POINT('Ctrl Pts',(5.56182083957535,-3.69825637721472,0.972043833535256));
#9047=CARTESIAN_POINT('Ctrl Pts',(5.68829012237594,-5.55779232620694,2.45913507001652));
#9048=CARTESIAN_POINT('Ctrl Pts',(5.8147594051765,-7.81890720937406,1.71302932929755));
#9049=CARTESIAN_POINT('Ctrl Pts',(5.94122868797707,-8.4282307243857,-0.588717647515425));
#9050=CARTESIAN_POINT('Ctrl Pts',(6.06769797077766,-6.83242220750502,-2.35583662162701));
#9051=CARTESIAN_POINT('Ctrl Pts',(6.19416725357822,-4.48067198566484,-1.98356630950483));
#9052=CARTESIAN_POINT('Ctrl Pts',(6.3206365363788,-3.50865839169727,0.190026077387566));
#9053=CARTESIAN_POINT('Ctrl Pts',(6.44710581917937,-4.79908927126543,2.19105142362198));
#9054=CARTESIAN_POINT('Ctrl Pts',(6.57357510197995,-7.1800947361798,2.20233270260992));
#9055=CARTESIAN_POINT('Ctrl Pts',(6.70004438478052,-8.4894290961712,0.213625126075533));
#9056=CARTESIAN_POINT('Ctrl Pts',(6.82651366758109,-7.53805577876764,-1.96908032866552));
#9057=CARTESIAN_POINT('Ctrl Pts',(6.95298295038167,-5.18993872094813,-2.36361876018877));
#9058=CARTESIAN_POINT('Ctrl Pts',(7.07945223318223,-3.57745689591113,-0.611700766905466));
#9059=CARTESIAN_POINT('Ctrl Pts',(7.20592151598281,-4.16494204432244,1.69571672710326));
#9060=CARTESIAN_POINT('Ctrl Pts',(7.33239079878337,-6.41888542408033,2.46321495627009));
#9061=CARTESIAN_POINT('Ctrl Pts',(7.45886008158396,-8.29242933985495,0.99381116993395));
#9062=CARTESIAN_POINT('Ctrl Pts',(7.58532936438452,-8.08416557645646,-1.37809534092029));
#9063=CARTESIAN_POINT('Ctrl Pts',(7.7117986471851,-5.98322323643802,-2.49852185490731));
#9064=CARTESIAN_POINT('Ctrl Pts',(7.83826792998567,-3.89751625931481,-1.34998334874579));
#9065=CARTESIAN_POINT('Ctrl Pts',(7.96473721278624,-3.72112300647373,1.02450600930416));
#9066=CARTESIAN_POINT('Ctrl Pts',(8.09120649558683,-5.61423023221168,2.46861795474968));
#9067=CARTESIAN_POINT('Ctrl Pts',(8.21767577838738,-7.8576638418784,1.67092129825785));
#9068=CARTESIAN_POINT('Ctrl Pts',(8.34414506118797,-8.41411028270966,-0.644177326125271));
#9069=CARTESIAN_POINT('Ctrl Pts',(8.47061434398854,-6.77824781455544,-2.37428373957647));
#9070=CARTESIAN_POINT('Ctrl Pts',(8.59708362678912,-4.43564060111505,-1.94824861894604));
#9071=CARTESIAN_POINT('Ctrl Pts',(8.72355290958969,-3.51366414375281,0.247035777478924));
#9072=CARTESIAN_POINT('Ctrl Pts',(8.85002219239026,-4.8495861402884,2.21798130490551));
#9073=CARTESIAN_POINT('Ctrl Pts',(8.97649147519083,-7.23022570399973,2.17472714445275));
#9074=CARTESIAN_POINT('Ctrl Pts',(9.1029607579914,-8.4936684162429,0.156553326289256));
#9075=CARTESIAN_POINT('Ctrl Pts',(9.22943004079198,-7.49255489929179,-2.00379007715825));
#9076=CARTESIAN_POINT('Ctrl Pts',(9.35589932359255,-5.13601559957201,-2.34444589565673));
#9077=CARTESIAN_POINT('Ctrl Pts',(9.48236860639313,-3.56408501733291,-0.55605630655366));
#9078=CARTESIAN_POINT('Ctrl Pts',(9.60883788919369,-4.20425579603823,1.73730019606714));
#9079=CARTESIAN_POINT('Ctrl Pts',(9.73530717199427,-6.47520016534523,2.45297563442673));
#9080=CARTESIAN_POINT('Ctrl Pts',(9.86177645479484,-8.31457166871008,0.9410455093623));
#9081=CARTESIAN_POINT('Ctrl Pts',(9.98824573759542,-8.05209011861891,-1.42546559228654));
#9082=CARTESIAN_POINT('Ctrl Pts',(10.114715020396,-5.92593865344554,-2.49748642043699));
#9083=CARTESIAN_POINT('Ctrl Pts',(10.2411843031966,-3.86727331938714,-1.30146772156772));
#9084=CARTESIAN_POINT('Ctrl Pts',(10.3676535859971,-3.7449469993049,1.07641531652463));
#9085=CARTESIAN_POINT('Ctrl Pts',(10.4941228687977,-5.67132678092312,2.47683529626786));
#9086=CARTESIAN_POINT('Ctrl Pts',(10.6205921515983,-7.89456967640777,1.62787928671148));
#9087=CARTESIAN_POINT('Ctrl Pts',(10.7470614343989,-8.40042620312697,-0.699181912156376));
#9088=CARTESIAN_POINT('Ctrl Pts',(10.8735307171994,-6.72017615484511,-2.39177453102291));
#9089=CARTESIAN_POINT('Ctrl Pts',(10.9578435723998,-5.1734383776302,-2.07118022033933));
#9090=CARTESIAN_POINT('Ctrl Pts',(11.,-4.63708777074269,-1.61992569438875));
#9091=CARTESIAN_POINT('Ctrl Pts',(0.710943720977493,-3.88529148023119,0.00143577679747337));
#9092=CARTESIAN_POINT('Ctrl Pts',(0.725958511702855,-3.88370462621288,0.251703649744779));
#9093=CARTESIAN_POINT('Ctrl Pts',(0.740973302428217,-3.92480148471753,0.50146841535006));
#9094=CARTESIAN_POINT('Ctrl Pts',(0.75598809315358,-4.01090210672623,0.7346104785572));
#9095=CARTESIAN_POINT('Ctrl Pts',(0.798144520753771,-4.25264338067621,1.38919412796826));
#9096=CARTESIAN_POINT('Ctrl Pts',(0.840300948353962,-4.84914728714184,1.91274176609648));
#9097=CARTESIAN_POINT('Ctrl Pts',(0.882457375954153,-5.52954858298102,2.0675566225593));
#9098=CARTESIAN_POINT('Ctrl Pts',(0.924613803554344,-6.2099498788202,2.22237147902212));
#9099=CARTESIAN_POINT('Ctrl Pts',(0.966770231154535,-6.97424856403293,2.00845355381954));
#9100=CARTESIAN_POINT('Ctrl Pts',(1.00892665875473,-7.47541430772541,1.52292113117499));
#9101=CARTESIAN_POINT('Ctrl Pts',(1.05108308635492,-7.9765800514179,1.03738870853044));
#9102=CARTESIAN_POINT('Ctrl Pts',(1.09323951395511,-8.21461285359015,0.280241788443912));
#9103=CARTESIAN_POINT('Ctrl Pts',(1.1353959415553,-8.08142687746697,-0.404721277761024));
#9104=CARTESIAN_POINT('Ctrl Pts',(1.17755236915549,-7.9482409013438,-1.08968434396596));
#9105=CARTESIAN_POINT('Ctrl Pts',(1.21970879675568,-7.44383614692521,-1.7024635562893));
#9106=CARTESIAN_POINT('Ctrl Pts',(1.26186522435587,-6.79724563204187,-1.96482319638538));
#9107=CARTESIAN_POINT('Ctrl Pts',(1.30402165195606,-6.15065511715852,-2.22718283648146));
#9108=CARTESIAN_POINT('Ctrl Pts',(1.34617807955626,-5.36187884181042,-2.13912290435027));
#9109=CARTESIAN_POINT('Ctrl Pts',(1.38833450715645,-4.78906854542857,-1.74062608291694));
#9110=CARTESIAN_POINT('Ctrl Pts',(1.4292042450968,-4.23374144502328,-1.35429209806172));
#9111=CARTESIAN_POINT('Ctrl Pts',(1.47007398303714,-3.88139817629141,-0.676182206719062));
#9112=CARTESIAN_POINT('Ctrl Pts',(1.51094372097749,-3.87968050865492,0.000387557652718817));
#9113=CARTESIAN_POINT('Ctrl Pts',(0.,-5.33826273143149,-2.47299490241842));
#9114=CARTESIAN_POINT('Ctrl Pts',(-2.92724693099176E-17,-5.25697989275057,
-2.4435642712672));
#9115=CARTESIAN_POINT('Ctrl Pts',(-2.99936341022307E-16,-5.17756935254689,
-2.40977678328915));
#9116=CARTESIAN_POINT('Ctrl Pts',(-1.89084858881472E-16,-5.10023122457203,
-2.37194495869841));
#9117=CARTESIAN_POINT('Ctrl Pts',(-7.18194080198928E-17,-5.01841824137493,
-2.33192414993816));
#9118=CARTESIAN_POINT('Ctrl Pts',(-4.57952225898383E-17,-4.93892346844573,
-2.28737700375529));
#9119=CARTESIAN_POINT('Ctrl Pts',(-1.42247325030098E-16,-4.86201628003916,
-2.2386224339937));
#9120=CARTESIAN_POINT('Ctrl Pts',(-2.26642914665326E-16,-4.79472249018341,
-2.19596218545231));
#9121=CARTESIAN_POINT('Ctrl Pts',(-2.00387407623276E-16,-4.7294100208876,
-2.1500794498512));
#9122=CARTESIAN_POINT('Ctrl Pts',(-2.35922392732846E-16,-4.66628671304646,
-2.10116352691532));
#9123=CARTESIAN_POINT('Ctrl Pts',(-2.53035131662012E-16,-4.6358881443092,
-2.07760687095783));
#9124=CARTESIAN_POINT('Ctrl Pts',(-3.2047257499942E-16,-4.60599768971522,
-2.0533464896154));
#9125=CARTESIAN_POINT('Ctrl Pts',(-3.19189119579733E-16,-4.57664107890252,
-2.02840217529484));
#9126=CARTESIAN_POINT('Ctrl Pts',(-3.1838209901331E-16,-4.55818201260159,
-2.0127175053303));
#9127=CARTESIAN_POINT('Ctrl Pts',(7.43895006162374E-17,-4.53993404802187,
-1.99676241071069));
#9128=CARTESIAN_POINT('Ctrl Pts',(8.32667268468867E-17,-4.52190394786633,
-1.98054167968357));
#9129=CARTESIAN_POINT('Ctrl Pts',(8.90116125221388E-17,-4.51023579146075,
-1.97004445421036));
#9130=CARTESIAN_POINT('Ctrl Pts',(7.79192238295981E-17,-4.4986578632022,
-1.95943488921183));
#9131=CARTESIAN_POINT('Ctrl Pts',(6.93889390390723E-17,-4.48718711125359,
-1.94872872076412));
#9132=CARTESIAN_POINT('Ctrl Pts',(2.2232716586874E-17,-4.4237757077816,
-1.88954400731919));
#9133=CARTESIAN_POINT('Ctrl Pts',(4.19397816253999E-17,-4.3635270875017,
-1.82731321714168));
#9134=CARTESIAN_POINT('Ctrl Pts',(-1.38777878078145E-17,-4.30667267111207,
-1.76231318129999));
#9135=CARTESIAN_POINT('Ctrl Pts',(-6.93621648361292E-17,-4.25015763638879,
-1.69770115085661));
#9136=CARTESIAN_POINT('Ctrl Pts',(2.58690954382853E-17,-4.19699589124401,
-1.63035201337592));
#9137=CARTESIAN_POINT('Ctrl Pts',(8.32667268468867E-17,-4.14745830932095,
-1.56051094849616));
#9138=CARTESIAN_POINT('Ctrl Pts',(1.34697385004543E-16,-4.10307058147718,
-1.49793045788973));
#9139=CARTESIAN_POINT('Ctrl Pts',(-9.33899128459785E-17,-4.061592963968,
-1.43334849733583));
#9140=CARTESIAN_POINT('Ctrl Pts',(-6.93889390390723E-17,-4.02325540423893,
-1.36693099493323));
#9141=CARTESIAN_POINT('Ctrl Pts',(-5.86560681904612E-17,-4.00611142997633,
-1.33723009691511));
#9142=CARTESIAN_POINT('Ctrl Pts',(7.82310118249411E-18,-3.98959585928372,
-1.30716204921597));
#9143=CARTESIAN_POINT('Ctrl Pts',(2.77555756156289E-17,-3.97373166622007,
-1.27674142037156));
#9144=CARTESIAN_POINT('Ctrl Pts',(3.74452042303345E-17,-3.9660197215955,
-1.26195326164511));
#9145=CARTESIAN_POINT('Ctrl Pts',(-9.49971474458872E-17,-3.95846173087556,
-1.24708178147702));
#9146=CARTESIAN_POINT('Ctrl Pts',(-1.11022302462516E-16,-3.95106046924767,
-1.23212865136607));
#9147=CARTESIAN_POINT('Ctrl Pts',(-1.24039512540166E-16,-3.94504843520807,
-1.21998224555778));
#9148=CARTESIAN_POINT('Ctrl Pts',(9.31053158590645E-17,-3.93913962598101,
-1.20778137348506));
#9149=CARTESIAN_POINT('Ctrl Pts',(8.32667268468867E-17,-3.93334209561816,
-1.19554126456453));
#9150=CARTESIAN_POINT('Ctrl Pts',(2.31250162516845E-17,-3.89790272592621,
-1.12071944941997));
#9151=CARTESIAN_POINT('Ctrl Pts',(-2.12799513447933E-16,-3.86655381569021,
-1.04430634320813));
#9152=CARTESIAN_POINT('Ctrl Pts',(-1.2490009027033E-16,-3.83953904065545,
-0.96652881623346));
#9153=CARTESIAN_POINT('Ctrl Pts',(-3.70006670927268E-17,-3.81252426562069,
-0.888751289258792));
#9154=CARTESIAN_POINT('Ctrl Pts',(-1.0547503387958E-16,-3.78984315653003,
-0.809608619610107));
#9155=CARTESIAN_POINT('Ctrl Pts',(-5.55111512312578E-17,-3.771792971052,
-0.729317871740391));
#9156=CARTESIAN_POINT('Ctrl Pts',(-3.97331530418015E-18,-3.75351269548682,
-0.648003638256219));
#9157=CARTESIAN_POINT('Ctrl Pts',(-7.84506068365862E-17,-3.73998283358267,
-0.565510657724717));
#9158=CARTESIAN_POINT('Ctrl Pts',(-1.66533453693773E-16,-3.73112919653385,
-0.482230005571742));
#9159=CARTESIAN_POINT('Ctrl Pts',(-1.95786173270394E-16,-3.72818886284729,
-0.454572116998511));
#9160=CARTESIAN_POINT('Ctrl Pts',(-1.59064674227402E-16,-3.7257646987008,
-0.426827461643137));
#9161=CARTESIAN_POINT('Ctrl Pts',(-1.66533453693773E-16,-3.72385518185906,
-0.399010789812195));
#9162=CARTESIAN_POINT('Ctrl Pts',(-1.70624142804513E-16,-3.72280932961687,
-0.383775454899953));
#9163=CARTESIAN_POINT('Ctrl Pts',(-4.49435376951814E-17,-3.72191787183054,
-0.368518521180014));
#9164=CARTESIAN_POINT('Ctrl Pts',(-5.55111512312578E-17,-3.72118063008209,
-0.353242451045553));
#9165=CARTESIAN_POINT('Ctrl Pts',(-6.45230566500116E-17,-3.72055192116072,
-0.34021524308114));
#9166=CARTESIAN_POINT('Ctrl Pts',(2.46893114276546E-16,-3.72003567571262,
-0.32717962863387));
#9167=CARTESIAN_POINT('Ctrl Pts',(2.4980018054066E-16,-3.71963163365472,
-0.314144903841315));
#9168=CARTESIAN_POINT('Ctrl Pts',(2.68015743063415E-16,-3.71709992206001,
-0.232469832530885));
#9169=CARTESIAN_POINT('Ctrl Pts',(5.488286943559E-16,-3.71896449420722,
-0.150735215678331));
#9170=CARTESIAN_POINT('Ctrl Pts',(4.44089209850063E-16,-3.72509763830452,
-0.0693027887965301));
#9171=CARTESIAN_POINT('Ctrl Pts',(3.39217825146735E-16,-3.73123850597352,
0.0122321873124179));
#9172=CARTESIAN_POINT('Ctrl Pts',(2.59200975553029E-16,-3.74165909148088,
0.093465234547049));
#9173=CARTESIAN_POINT('Ctrl Pts',(3.33066907387547E-16,-3.75628187779841,
0.174020871474803));
#9174=CARTESIAN_POINT('Ctrl Pts',(4.05749365005722E-16,-3.77067037897056,
0.253285852251375));
#9175=CARTESIAN_POINT('Ctrl Pts',(1.15570041343854E-16,-3.7891279795921,
0.331895826436378));
#9176=CARTESIAN_POINT('Ctrl Pts',(8.32667268468867E-17,-3.81162326334501,
0.409467154655233));
#9177=CARTESIAN_POINT('Ctrl Pts',(7.02983539418161E-17,-3.82065413936675,
0.440608662167665));
#9178=CARTESIAN_POINT('Ctrl Pts',(-1.41317173045025E-16,-3.83033620254681,
0.471582407310852));
#9179=CARTESIAN_POINT('Ctrl Pts',(-1.66533453693773E-16,-3.84066913389938,
0.502361889653307));
#9180=CARTESIAN_POINT('Ctrl Pts',(-1.78089117460353E-16,-3.84540432391796,
0.516466957478861));
#9181=CARTESIAN_POINT('Ctrl Pts',(-1.91790833069298E-16,-3.85027647415249,
0.530531683564752));
#9182=CARTESIAN_POINT('Ctrl Pts',(-1.66533453693773E-16,-3.85528015633242,
0.544538943406607));
#9183=CARTESIAN_POINT('Ctrl Pts',(-3.24796012030796E-17,-3.88183726120405,
0.618882647744295));
#9184=CARTESIAN_POINT('Ctrl Pts',(2.04582574808049E-16,-3.91212927413511,
0.691710442324472));
#9185=CARTESIAN_POINT('Ctrl Pts',(3.88578058618805E-16,-3.94610117464232,
0.762666157003909));
#9186=CARTESIAN_POINT('Ctrl Pts',(5.25025058613771E-16,-3.97129398814151,
0.815285352866705));
#9187=CARTESIAN_POINT('Ctrl Pts',(3.51076268717821E-16,-3.99851141404213,
0.866874595241459));
#9188=CARTESIAN_POINT('Ctrl Pts',(3.60822483003176E-16,-4.02774432096395,
0.917275939864036));
#9189=CARTESIAN_POINT('Ctrl Pts',(3.64283941088971E-16,-4.03812665805127,
0.93517644325651));
#9190=CARTESIAN_POINT('Ctrl Pts',(1.25791190295242E-16,-4.04876332126932,
0.952926991687769));
#9191=CARTESIAN_POINT('Ctrl Pts',(1.11022302462516E-16,-4.05965421258269,
0.970520102081179));
#9192=CARTESIAN_POINT('Ctrl Pts',(1.00739750509289E-16,-4.06723678460943,
0.982768964262814));
#9193=CARTESIAN_POINT('Ctrl Pts',(2.31163055125436E-16,-4.07494162572207,
0.994939826680167));
#9194=CARTESIAN_POINT('Ctrl Pts',(2.4980018054066E-16,-4.08276363356959,
1.00702274898775));
#9195=CARTESIAN_POINT('Ctrl Pts',(3.47541887158804E-16,-4.12378586093371,
1.0703911827438));
#9196=CARTESIAN_POINT('Ctrl Pts',(3.68255127129089E-16,-4.16806493610171,
1.13140389034015));
#9197=CARTESIAN_POINT('Ctrl Pts',(4.44089209850063E-16,-4.21556997754234,
1.1897206136822));
#9198=CARTESIAN_POINT('Ctrl Pts',(5.08458397066477E-16,-4.25589301959016,
1.23922078495035));
#9199=CARTESIAN_POINT('Ctrl Pts',(7.76827601613562E-17,-4.29854102111365,
1.28677822183849));
#9200=CARTESIAN_POINT('Ctrl Pts',(5.55111512312578E-17,-4.34351204228601,
1.33216059575643));
#9201=CARTESIAN_POINT('Ctrl Pts',(5.00618174492108E-17,-4.35456501122752,
1.3433146668967));
#9202=CARTESIAN_POINT('Ctrl Pts',(-1.66995712675634E-17,-4.3657583778192,
1.35433722656524));
#9203=CARTESIAN_POINT('Ctrl Pts',(0.,-4.3770892093283,1.36522705282965));
#9204=CARTESIAN_POINT('Origin',(6.,-6.,0.));
#9205=CARTESIAN_POINT('Origin',(12.,-6.,0.));
#9206=CARTESIAN_POINT('Origin',(12.,6.,0.));
#9207=CARTESIAN_POINT('Origin',(80.,-7.,-6.));
#9208=CARTESIAN_POINT('',(80.,-7.,-6.));
#9209=CARTESIAN_POINT('',(20.,-7.,-6.));
#9210=CARTESIAN_POINT('',(20.,-7.,-6.));
#9211=CARTESIAN_POINT('',(20.,-7.,6.));
#9212=CARTESIAN_POINT('',(20.,-7.,-6.));
#9213=CARTESIAN_POINT('',(80.,-7.,6.));
#9214=CARTESIAN_POINT('',(20.,-7.,6.));
#9215=CARTESIAN_POINT('',(80.,-7.,-6.));
#9216=CARTESIAN_POINT('Origin',(80.,-5.00000000000001,-6.));
#9217=CARTESIAN_POINT('',(82.,-5.,-6.));
#9218=CARTESIAN_POINT('Origin',(80.,-5.00000000000001,-6.));
#9219=CARTESIAN_POINT('',(82.,-5.,6.));
#9220=CARTESIAN_POINT('Origin',(80.,-5.00000000000001,6.));
#9221=CARTESIAN_POINT('',(82.,-5.,-6.));
#9222=CARTESIAN_POINT('Origin',(82.,5.,-6.));
#9223=CARTESIAN_POINT('',(82.,5.,-6.));
#9224=CARTESIAN_POINT('',(82.,-5.,-6.));
#9225=CARTESIAN_POINT('',(82.,5.,6.));
#9226=CARTESIAN_POINT('',(82.,-5.,6.));
#9227=CARTESIAN_POINT('',(82.,5.,-6.));
#9228=CARTESIAN_POINT('Origin',(80.,5.00000000000001,-6.));
#9229=CARTESIAN_POINT('',(80.,7.,-6.));
#9230=CARTESIAN_POINT('Origin',(80.,5.00000000000001,-6.));
#9231=CARTESIAN_POINT('',(80.,7.,6.));
#9232=CARTESIAN_POINT('Origin',(80.,5.00000000000001,6.));
#9233=CARTESIAN_POINT('',(80.,7.,-6.));
#9234=CARTESIAN_POINT('Origin',(20.,7.,-6.));
#9235=CARTESIAN_POINT('',(20.,7.,-6.));
#9236=CARTESIAN_POINT('',(80.,7.,-6.));
#9237=CARTESIAN_POINT('',(20.,7.,6.));
#9238=CARTESIAN_POINT('',(80.,7.,6.));
#9239=CARTESIAN_POINT('',(20.,7.,-6.));
#9240=CARTESIAN_POINT('Origin',(20.,5.,-6.));
#9241=CARTESIAN_POINT('',(18.,5.,-6.));
#9242=CARTESIAN_POINT('Origin',(20.,5.,-6.));
#9243=CARTESIAN_POINT('',(18.,5.,6.));
#9244=CARTESIAN_POINT('Origin',(20.,5.,6.));
#9245=CARTESIAN_POINT('',(18.,5.,-6.));
#9246=CARTESIAN_POINT('Origin',(18.,-5.,-6.));
#9247=CARTESIAN_POINT('',(18.,-5.,-6.));
#9248=CARTESIAN_POINT('',(18.,5.,-6.));
#9249=CARTESIAN_POINT('',(18.,-5.,6.));
#9250=CARTESIAN_POINT('',(18.,5.,6.));
#9251=CARTESIAN_POINT('',(18.,-5.,-6.));
#9252=CARTESIAN_POINT('Origin',(20.,-5.,-6.));
#9253=CARTESIAN_POINT('Origin',(20.,-5.,-6.));
#9254=CARTESIAN_POINT('Origin',(20.,-5.,6.));
#9255=CARTESIAN_POINT('Origin',(22.,10.,-6.));
#9256=CARTESIAN_POINT('',(20.,10.,-6.));
#9257=CARTESIAN_POINT('',(22.,8.,-6.));
#9258=CARTESIAN_POINT('Origin',(22.,10.,-6.));
#9259=CARTESIAN_POINT('',(20.,10.,6.));
#9260=CARTESIAN_POINT('',(20.,10.,-6.));
#9261=CARTESIAN_POINT('',(22.,8.,6.));
#9262=CARTESIAN_POINT('Origin',(22.,10.,6.));
#9263=CARTESIAN_POINT('',(22.,8.,-6.));
#9264=CARTESIAN_POINT('Origin',(78.,8.,-6.));
#9265=CARTESIAN_POINT('',(78.,8.,-6.));
#9266=CARTESIAN_POINT('',(78.,8.,-6.));
#9267=CARTESIAN_POINT('',(78.,8.,6.));
#9268=CARTESIAN_POINT('',(78.,8.,6.));
#9269=CARTESIAN_POINT('',(78.,8.,-6.));
#9270=CARTESIAN_POINT('Origin',(78.,10.,-6.));
#9271=CARTESIAN_POINT('',(80.,10.,-6.));
#9272=CARTESIAN_POINT('Origin',(78.,10.,-6.));
#9273=CARTESIAN_POINT('',(80.,10.,6.));
#9274=CARTESIAN_POINT('Origin',(78.,10.,6.));
#9275=CARTESIAN_POINT('',(80.,10.,-6.));
#9276=CARTESIAN_POINT('Origin',(80.,12.,-6.));
#9277=CARTESIAN_POINT('',(80.,12.,-6.));
#9278=CARTESIAN_POINT('',(80.,12.,-6.));
#9279=CARTESIAN_POINT('',(80.,12.,6.));
#9280=CARTESIAN_POINT('',(80.,12.,6.));
#9281=CARTESIAN_POINT('',(80.,12.,-6.));
#9282=CARTESIAN_POINT('Origin',(96.,12.,-6.));
#9283=CARTESIAN_POINT('',(96.,12.,-6.));
#9284=CARTESIAN_POINT('',(96.,12.,-6.));
#9285=CARTESIAN_POINT('',(96.,12.,6.));
#9286=CARTESIAN_POINT('',(96.,12.,6.));
#9287=CARTESIAN_POINT('',(96.,12.,-6.));
#9288=CARTESIAN_POINT('Origin',(96.,-12.,-6.));
#9289=CARTESIAN_POINT('',(96.,-12.,-6.));
#9290=CARTESIAN_POINT('',(96.,-12.,-6.));
#9291=CARTESIAN_POINT('',(96.,-12.,6.));
#9292=CARTESIAN_POINT('',(96.,-12.,6.));
#9293=CARTESIAN_POINT('',(96.,-12.,-6.));
#9294=CARTESIAN_POINT('Origin',(80.,-12.,-6.));
#9295=CARTESIAN_POINT('',(80.,-12.,-6.));
#9296=CARTESIAN_POINT('',(80.,-12.,-6.));
#9297=CARTESIAN_POINT('',(80.,-12.,6.));
#9298=CARTESIAN_POINT('',(80.,-12.,6.));
#9299=CARTESIAN_POINT('',(80.,-12.,-6.));
#9300=CARTESIAN_POINT('Origin',(80.,-10.,-6.));
#9301=CARTESIAN_POINT('',(80.,-10.,-6.));
#9302=CARTESIAN_POINT('',(80.,-10.,-6.));
#9303=CARTESIAN_POINT('',(80.,-10.,6.));
#9304=CARTESIAN_POINT('',(80.,-10.,6.));
#9305=CARTESIAN_POINT('',(80.,-10.,-6.));
#9306=CARTESIAN_POINT('Origin',(78.,-10.,-6.));
#9307=CARTESIAN_POINT('',(78.,-8.,-6.));
#9308=CARTESIAN_POINT('Origin',(78.,-10.,-6.));
#9309=CARTESIAN_POINT('',(78.,-8.,6.));
#9310=CARTESIAN_POINT('Origin',(78.,-10.,6.));
#9311=CARTESIAN_POINT('',(78.,-8.,-6.));
#9312=CARTESIAN_POINT('Origin',(22.,-8.,-6.));
#9313=CARTESIAN_POINT('',(22.,-8.,-6.));
#9314=CARTESIAN_POINT('',(22.,-8.,-6.));
#9315=CARTESIAN_POINT('',(22.,-8.,6.));
#9316=CARTESIAN_POINT('',(22.,-8.,6.));
#9317=CARTESIAN_POINT('',(22.,-8.,-6.));
#9318=CARTESIAN_POINT('Origin',(22.,-10.,-6.));
#9319=CARTESIAN_POINT('',(20.,-10.,-6.));
#9320=CARTESIAN_POINT('Origin',(22.,-10.,-6.));
#9321=CARTESIAN_POINT('',(20.,-10.,6.));
#9322=CARTESIAN_POINT('Origin',(22.,-10.,6.));
#9323=CARTESIAN_POINT('',(20.,-10.,-6.));
#9324=CARTESIAN_POINT('Origin',(20.,-12.,-6.));
#9325=CARTESIAN_POINT('',(20.,-12.,-6.));
#9326=CARTESIAN_POINT('',(20.,-12.,-6.));
#9327=CARTESIAN_POINT('',(20.,-12.,6.));
#9328=CARTESIAN_POINT('',(20.,-12.,6.));
#9329=CARTESIAN_POINT('',(20.,-12.,-6.));
#9330=CARTESIAN_POINT('Origin',(0.,-12.,-6.));
#9331=CARTESIAN_POINT('',(0.,-12.,-6.));
#9332=CARTESIAN_POINT('',(0.,-12.,-6.));
#9333=CARTESIAN_POINT('',(0.,-12.,6.));
#9334=CARTESIAN_POINT('',(0.,-12.,6.));
#9335=CARTESIAN_POINT('',(0.,-12.,-6.));
#9336=CARTESIAN_POINT('Origin',(0.,12.,-6.));
#9337=CARTESIAN_POINT('',(0.,12.,-6.));
#9338=CARTESIAN_POINT('',(0.,12.,-6.));
#9339=CARTESIAN_POINT('',(0.,12.,6.));
#9340=CARTESIAN_POINT('',(0.,12.,6.));
#9341=CARTESIAN_POINT('',(0.,12.,-6.));
#9342=CARTESIAN_POINT('Origin',(20.,12.,-6.));
#9343=CARTESIAN_POINT('',(20.,12.,-6.));
#9344=CARTESIAN_POINT('',(20.,12.,-6.));
#9345=CARTESIAN_POINT('',(20.,12.,6.));
#9346=CARTESIAN_POINT('',(20.,12.,6.));
#9347=CARTESIAN_POINT('',(20.,12.,-6.));
#9348=CARTESIAN_POINT('Origin',(20.,10.,-6.));
#9349=CARTESIAN_POINT('',(20.,10.,-6.));
#9350=CARTESIAN_POINT('',(20.,10.,6.));
#9351=CARTESIAN_POINT('Origin',(48.,0.,6.));
#9352=CARTESIAN_POINT('Origin',(48.,0.,-6.));
#9353=CARTESIAN_POINT('',(0.,0.,0.));
#9354=CARTESIAN_POINT('Origin',(94.,-12.,-5.));
#9355=CARTESIAN_POINT('',(94.,-12.,-5.));
#9356=CARTESIAN_POINT('',(84.,-12.,-5.));
#9357=CARTESIAN_POINT('',(94.,-12.,-5.));
#9358=CARTESIAN_POINT('',(84.,-12.,5.));
#9359=CARTESIAN_POINT('',(84.,-12.,-5.));
#9360=CARTESIAN_POINT('',(94.,-12.,5.));
#9361=CARTESIAN_POINT('',(94.,-12.,5.));
#9362=CARTESIAN_POINT('',(94.,-12.,-5.));
#9363=CARTESIAN_POINT('Origin',(94.,-14.,-5.));
#9364=CARTESIAN_POINT('',(94.,-14.,-5.));
#9365=CARTESIAN_POINT('',(94.,-14.,-5.));
#9366=CARTESIAN_POINT('',(94.,-14.,5.));
#9367=CARTESIAN_POINT('',(94.,-14.,5.));
#9368=CARTESIAN_POINT('',(94.,-14.,-5.));
#9369=CARTESIAN_POINT('Origin',(84.,-14.,-5.));
#9370=CARTESIAN_POINT('',(84.,-14.,-5.));
#9371=CARTESIAN_POINT('',(84.,-14.,-5.));
#9372=CARTESIAN_POINT('',(84.,-14.,5.));
#9373=CARTESIAN_POINT('',(84.,-14.,5.));
#9374=CARTESIAN_POINT('',(84.,-14.,-5.));
#9375=CARTESIAN_POINT('Origin',(84.,-12.,-5.));
#9376=CARTESIAN_POINT('',(84.,-12.,-5.));
#9377=CARTESIAN_POINT('',(84.,-12.,5.));
#9378=CARTESIAN_POINT('Origin',(89.,-13.,5.));
#9379=CARTESIAN_POINT('Origin',(89.,-13.,-5.));
#9380=CARTESIAN_POINT('',(0.,0.,0.));
#9381=CARTESIAN_POINT('Origin',(0.,0.,0.));
#9382=CARTESIAN_POINT('',(-3.,-3.67394039744206E-16,2.));
#9383=CARTESIAN_POINT('Origin',(0.,0.,2.));
#9384=CARTESIAN_POINT('',(-3.,-3.67394039744206E-16,0.));
#9385=CARTESIAN_POINT('',(-3.,-3.67394039744206E-16,0.));
#9386=CARTESIAN_POINT('Origin',(0.,0.,0.));
#9387=CARTESIAN_POINT('Origin',(0.,0.,0.));
#9388=CARTESIAN_POINT('',(-6.,-7.34788079488412E-16,2.));
#9389=CARTESIAN_POINT('Origin',(0.,0.,2.));
#9390=CARTESIAN_POINT('',(-6.,-7.34788079488412E-16,0.));
#9391=CARTESIAN_POINT('',(-6.,-7.34788079488412E-16,0.));
#9392=CARTESIAN_POINT('Origin',(0.,0.,0.));
#9393=CARTESIAN_POINT('Origin',(0.,0.,2.));
#9394=CARTESIAN_POINT('Origin',(0.,0.,0.));
#9395=CARTESIAN_POINT('',(0.,0.,0.));
#9396=CARTESIAN_POINT('Origin',(0.,0.,0.));
#9397=CARTESIAN_POINT('',(-2.45343712965594,0.00158941762237803,0.257827496212055));
#9398=CARTESIAN_POINT('',(-2.45278840085115,0.00262419282126472,0.142172503787962));
#9399=CARTESIAN_POINT('',(-2.4505,-3.00099698131059E-16,0.));
#9400=CARTESIAN_POINT('',(1.07508846035129,2.20207516956608,0.));
#9401=CARTESIAN_POINT('Ctrl Pts',(-2.45343712965594,0.00158941762237803,
0.257827496212055));
#9402=CARTESIAN_POINT('Ctrl Pts',(-2.4540150018513,0.085172055481945,0.253469478752161));
#9403=CARTESIAN_POINT('Ctrl Pts',(-2.45011475290023,0.168696598429799,0.249111461292266));
#9404=CARTESIAN_POINT('Ctrl Pts',(-2.44155870478254,0.251737029249849,0.244753443832372));
#9405=CARTESIAN_POINT('Ctrl Pts',(-2.35846563071267,1.05819400261022,0.20243004141441));
#9406=CARTESIAN_POINT('Ctrl Pts',(-1.83625838436405,1.81899168340171,0.160106638996448));
#9407=CARTESIAN_POINT('Ctrl Pts',(-1.11361254088691,2.18710613238446,0.117783236578486));
#9408=CARTESIAN_POINT('Ctrl Pts',(-0.443253972640013,2.52858554058766,0.0785221577189908));
#9409=CARTESIAN_POINT('Ctrl Pts',(0.399586947667411,2.53215135127315,0.0392610788594954));
#9410=CARTESIAN_POINT('Ctrl Pts',(1.07765127757232,2.20530172674001,-6.18615037552163E-17));
#9411=CARTESIAN_POINT('',(-1.0750884603512,2.20207516956613,0.));
#9412=CARTESIAN_POINT('Origin',(0.,0.,0.));
#9413=CARTESIAN_POINT('Ctrl Pts',(-1.0750884603512,2.20207516956613,-4.75314232417645E-15));
#9414=CARTESIAN_POINT('Ctrl Pts',(-1.8073457627734,1.84457539538852,0.042339106641334));
#9415=CARTESIAN_POINT('Ctrl Pts',(-2.34095039172362,1.09624395863826,0.0846782132826726));
#9416=CARTESIAN_POINT('Ctrl Pts',(-2.43687977559142,0.292153052631133,0.127017319924011));
#9417=CARTESIAN_POINT('Ctrl Pts',(-2.44832567486989,0.196212235023275,0.132069047878662));
#9418=CARTESIAN_POINT('Ctrl Pts',(-2.45354070668951,0.0994776099830367,
0.137120775833312));
#9419=CARTESIAN_POINT('Ctrl Pts',(-2.45278840085115,0.00262419282126472,
0.142172503787962));
#9420=CARTESIAN_POINT('Origin',(0.,0.,0.));
#9421=CARTESIAN_POINT('',(-2.44709082993613,0.00122547174869078,1.05782749621206));
#9422=CARTESIAN_POINT('',(-2.4469182083441,0.00108108736496512,0.942172503787958));
#9423=CARTESIAN_POINT('',(-2.4505,-3.00099698131059E-16,0.));
#9424=CARTESIAN_POINT('Ctrl Pts',(-2.44709082993613,0.00122547174869078,
1.05782749621206));
#9425=CARTESIAN_POINT('Ctrl Pts',(-2.44858147013302,0.331094139137146,1.04074322659327));
#9426=CARTESIAN_POINT('Ctrl Pts',(-2.38654629113948,0.660424866872034,1.02365895697448));
#9427=CARTESIAN_POINT('Ctrl Pts',(-2.25832126611665,0.961571221090581,1.00657468735569));
#9428=CARTESIAN_POINT('Ctrl Pts',(-1.9406653489959,1.70761062579985,0.964251284937728));
#9429=CARTESIAN_POINT('Ctrl Pts',(-1.21679094422775,2.28067767489988,0.921927882519764));
#9430=CARTESIAN_POINT('Ctrl Pts',(-0.417767228755014,2.41869275133695,0.879604480101802));
#9431=CARTESIAN_POINT('Ctrl Pts',(0.381256486717722,2.55670782777402,0.83728107768384));
#9432=CARTESIAN_POINT('Ctrl Pts',(1.25542951289504,2.25967093154815,0.794957675265879));
#9433=CARTESIAN_POINT('Ctrl Pts',(1.80493193792011,1.66339843739796,0.752634272847918));
#9434=CARTESIAN_POINT('Ctrl Pts',(2.35443436294518,1.06712594324778,0.710310870429956));
#9435=CARTESIAN_POINT('Ctrl Pts',(2.57926618681799,0.171617851173292,0.667987468011993));
#9436=CARTESIAN_POINT('Ctrl Pts',(2.37661022655832,-0.613484110704425,0.625664065594031));
#9437=CARTESIAN_POINT('Ctrl Pts',(2.17395426629865,-1.39858607258214,0.583340663176068));
#9438=CARTESIAN_POINT('Ctrl Pts',(1.5438105219065,-2.07328190426309,0.541017260758106));
#9439=CARTESIAN_POINT('Ctrl Pts',(0.774359256385592,-2.32912561010772,0.498693858340144));
#9440=CARTESIAN_POINT('Ctrl Pts',(0.00490799086468277,-2.58496931595236,
0.456370455922182));
#9441=CARTESIAN_POINT('Ctrl Pts',(-0.903850795784982,-2.42196089596069,
0.41404705350422));
#9442=CARTESIAN_POINT('Ctrl Pts',(-1.53624073821425,-1.91439855300023,0.371723651086258));
#9443=CARTESIAN_POINT('Ctrl Pts',(-2.1035138362237,-1.45909962522464,0.33375826612819));
#9444=CARTESIAN_POINT('Ctrl Pts',(-2.44840292762362,-0.726550625723455,
0.295792881170123));
#9445=CARTESIAN_POINT('Ctrl Pts',(-2.45343712965594,0.00158941762237803,
0.257827496212055));
#9446=CARTESIAN_POINT('Ctrl Pts',(-2.45278840085115,0.00262419282126472,
0.142172503787962));
#9447=CARTESIAN_POINT('Ctrl Pts',(-2.44723554588049,-0.712261896697142,
0.179459882474651));
#9448=CARTESIAN_POINT('Ctrl Pts',(-2.11657712126492,-1.43361988081142,0.216747261161339));
#9449=CARTESIAN_POINT('Ctrl Pts',(-1.56678617588997,-1.89000633907613,0.254034639848028));
#9450=CARTESIAN_POINT('Ctrl Pts',(-0.942509053535351,-2.40822444951227,
0.296373746489366));
#9451=CARTESIAN_POINT('Ctrl Pts',(-0.0357006700407422,-2.58481029512054,
0.338712853130705));
#9452=CARTESIAN_POINT('Ctrl Pts',(0.738006177904425,-2.34071471461417,0.381051959772044));
#9453=CARTESIAN_POINT('Ctrl Pts',(1.51171302584959,-2.09661913410779,0.423391066413383));
#9454=CARTESIAN_POINT('Ctrl Pts',(2.15231833824532,-1.43184212748677,0.465730173054722));
#9455=CARTESIAN_POINT('Ctrl Pts',(2.3669503643466,-0.649736793975562,0.508069279696061));
#9456=CARTESIAN_POINT('Ctrl Pts',(2.58158239044788,0.132368539535648,0.550408386337399));
#9457=CARTESIAN_POINT('Ctrl Pts',(2.37024113025471,1.03180219993705,0.592747492978738));
#9458=CARTESIAN_POINT('Ctrl Pts',(1.82948647714086,1.63645052880757,0.635086599620077));
#9459=CARTESIAN_POINT('Ctrl Pts',(1.28873182402701,2.24109885767809,0.677425706261415));
#9460=CARTESIAN_POINT('Ctrl Pts',(0.418563777992485,2.55096185501775,0.719764812902754));
#9461=CARTESIAN_POINT('Ctrl Pts',(-0.382678773049915,2.42446863484039,0.762103919544093));
#9462=CARTESIAN_POINT('Ctrl Pts',(-1.18392132409231,2.29797541466303,0.804443026185432));
#9463=CARTESIAN_POINT('Ctrl Pts',(-1.91623838014258,1.73512597696867,0.846782132826771));
#9464=CARTESIAN_POINT('Ctrl Pts',(-2.24451388823343,0.993392607903086,0.88912123946811));
#9465=CARTESIAN_POINT('Ctrl Pts',(-2.381624565422,0.683593180229046,0.906804994241392));
#9466=CARTESIAN_POINT('Ctrl Pts',(-2.44825106878348,0.342587837773907,0.924488749014675));
#9467=CARTESIAN_POINT('Ctrl Pts',(-2.4469182083441,0.00108108736496512,
0.942172503787958));
#9468=CARTESIAN_POINT('Origin',(0.,0.,0.));
#9469=CARTESIAN_POINT('',(-2.44901144034399,-0.00211142026644101,1.85782749621206));
#9470=CARTESIAN_POINT('',(-2.44927322928455,-0.00216311090478056,1.74217250378796));
#9471=CARTESIAN_POINT('',(-2.4505,-3.00099698131059E-16,0.));
#9472=CARTESIAN_POINT('Ctrl Pts',(-2.44901144034399,-0.00211142026644101,
1.85782749621206));
#9473=CARTESIAN_POINT('Ctrl Pts',(-2.44428079907938,0.572343309026032,1.82801697443437));
#9474=CARTESIAN_POINT('Ctrl Pts',(-2.24249780427236,1.14979088066879,1.79820645265669));
#9475=CARTESIAN_POINT('Ctrl Pts',(-1.87352390546256,1.58572983322239,1.76839593087901));
#9476=CARTESIAN_POINT('Ctrl Pts',(-1.34967427553953,2.2046529052903,1.72607252846104));
#9477=CARTESIAN_POINT('Ctrl Pts',(-0.488820969467413,2.5383396176156,1.68374912604308));
#9478=CARTESIAN_POINT('Ctrl Pts',(0.315314577443851,2.43417478721053,1.64142572362512));
#9479=CARTESIAN_POINT('Ctrl Pts',(1.11945012435512,2.33000995680546,1.59910232120716));
#9480=CARTESIAN_POINT('Ctrl Pts',(1.86686791210553,1.78799358367002,1.5567789187892));
#9481=CARTESIAN_POINT('Ctrl Pts',(2.21572738312456,1.05602253293468,1.51445551637123));
#9482=CARTESIAN_POINT('Ctrl Pts',(2.56458685414359,0.324051482199336,1.47213211395327));
#9483=CARTESIAN_POINT('Ctrl Pts',(2.51488800843124,-0.597874246135909,1.42980871153531));
#9484=CARTESIAN_POINT('Ctrl Pts',(2.08936146294263,-1.28809947042103,1.38748530911735));
#9485=CARTESIAN_POINT('Ctrl Pts',(1.66383491745404,-1.97832469470614,1.34516190669938));
#9486=CARTESIAN_POINT('Ctrl Pts',(0.862480672189199,-2.43684941494112,1.30283850428142));
#9487=CARTESIAN_POINT('Ctrl Pts',(0.0518071380387072,-2.45396470323855,
1.26051510186346));
#9488=CARTESIAN_POINT('Ctrl Pts',(-0.758866396111789,-2.47107999153598,
1.2181916994455));
#9489=CARTESIAN_POINT('Ctrl Pts',(-1.57885921914794,-2.04678584789584,1.17586829702754));
#9490=CARTESIAN_POINT('Ctrl Pts',(-2.03313691592934,-1.37513289591652,1.13354489460957));
#9491=CARTESIAN_POINT('Ctrl Pts',(-2.30404082397389,-0.974599453861103,
1.1083057618104));
#9492=CARTESIAN_POINT('Ctrl Pts',(-2.44488865994441,-0.486099962014506,
1.08306662901123));
#9493=CARTESIAN_POINT('Ctrl Pts',(-2.44709082993613,0.00122547174869078,
1.05782749621206));
#9494=CARTESIAN_POINT('Ctrl Pts',(-2.4469182083441,0.00108108736496512,
0.942172503787958));
#9495=CARTESIAN_POINT('Ctrl Pts',(-2.4450598845014,-0.475060388503602,0.966827855656014));
#9496=CARTESIAN_POINT('Ctrl Pts',(-2.31109549859399,-0.952176550222066,
0.99148320752407));
#9497=CARTESIAN_POINT('Ctrl Pts',(-2.05186792976456,-1.34705035287639,1.01613855939213));
#9498=CARTESIAN_POINT('Ctrl Pts',(-1.60671250307345,-2.02514264415345,1.05847766603346));
#9499=CARTESIAN_POINT('Ctrl Pts',(-0.792167689559793,-2.46070992627076,
1.1008167726748));
#9500=CARTESIAN_POINT('Ctrl Pts',(0.018959005881323,-2.45444035901399,1.14315587931614));
#9501=CARTESIAN_POINT('Ctrl Pts',(0.830085701322441,-2.44817079175722,1.18549498595748));
#9502=CARTESIAN_POINT('Ctrl Pts',(1.63779427869103,-2.00006437512636,1.22783409259882));
#9503=CARTESIAN_POINT('Ctrl Pts',(2.07242512020182,-1.31518860000204,1.27017319924016));
#9504=CARTESIAN_POINT('Ctrl Pts',(2.50705596171262,-0.630312824877714,1.3125123058815));
#9505=CARTESIAN_POINT('Ctrl Pts',(2.56860906736563,0.29133230874007,1.35485141252284));
#9506=CARTESIAN_POINT('Ctrl Pts',(2.22890980083579,1.02792517390474,1.39719051916417));
#9507=CARTESIAN_POINT('Ctrl Pts',(1.88921053430595,1.76451803906942,1.43952962580551));
#9508=CARTESIAN_POINT('Ctrl Pts',(1.14825889559327,2.31605863578098,1.48186873244685));
#9509=CARTESIAN_POINT('Ctrl Pts',(0.345170071483936,2.43012699230601,1.52420783908819));
#9510=CARTESIAN_POINT('Ctrl Pts',(-0.457918752625402,2.54419534883104,1.56654694572953));
#9511=CARTESIAN_POINT('Ctrl Pts',(-1.32314476213139,2.22079146516954,1.60888605237087));
#9512=CARTESIAN_POINT('Ctrl Pts',(-1.85451854586612,1.60792579269655,1.65122515901221));
#9513=CARTESIAN_POINT('Ctrl Pts',(-2.23499448995806,1.16909976763974,1.68154094060412));
#9514=CARTESIAN_POINT('Ctrl Pts',(-2.44430800748012,0.581869813096559,1.71185672219604));
#9515=CARTESIAN_POINT('Ctrl Pts',(-2.44927322928455,-0.00216311090478056,
1.74217250378796));
#9516=CARTESIAN_POINT('Origin',(0.,0.,0.));
#9517=CARTESIAN_POINT('',(-2.45450932558232,7.6261763116035E-5,2.65782749621206));
#9518=CARTESIAN_POINT('',(-2.45449494699467,0.000217524429918226,2.54217250378796));
#9519=CARTESIAN_POINT('',(-2.4505,-3.00099698131059E-16,0.));
#9520=CARTESIAN_POINT('Ctrl Pts',(-2.45450932558232,7.6261763116035E-5,
2.65782749621206));
#9521=CARTESIAN_POINT('Ctrl Pts',(-2.45451119120266,0.00416415927192646,
2.65761412469344));
#9522=CARTESIAN_POINT('Ctrl Pts',(-2.45450186106136,0.00825204801413194,
2.65740075317482));
#9523=CARTESIAN_POINT('Ctrl Pts',(-2.45448130952338,0.0123398803409236,
2.65718738165621));
#9524=CARTESIAN_POINT('Ctrl Pts',(-2.45040480007216,0.823183678550061,2.61486397923825));
#9525=CARTESIAN_POINT('Ctrl Pts',(-2.00482375815798,1.63180781893863,2.57254057682028));
#9526=CARTESIAN_POINT('Ctrl Pts',(-1.32152997796213,2.06837842113986,2.53021717440232));
#9527=CARTESIAN_POINT('Ctrl Pts',(-0.638236197766273,2.50494902334109,2.48789377198436));
#9528=CARTESIAN_POINT('Ctrl Pts',(0.282770320711254,2.56946608735497,2.4455703695664));
#9529=CARTESIAN_POINT('Ctrl Pts',(1.02025628473274,2.23242197451411,2.40324696714844));
#9530=CARTESIAN_POINT('Ctrl Pts',(1.75774224875421,1.89537786167325,2.36092356473047));
#9531=CARTESIAN_POINT('Ctrl Pts',(2.31170765831966,1.15677257197763,2.31860016231251));
#9532=CARTESIAN_POINT('Ctrl Pts',(2.42878983651432,0.354416010264148,2.27627675989455));
#9533=CARTESIAN_POINT('Ctrl Pts',(2.54587201470898,-0.447940551449347,2.23395335747659));
#9534=CARTESIAN_POINT('Ctrl Pts',(2.22607096153286,-1.31404838518072,2.19162995505863));
#9535=CARTESIAN_POINT('Ctrl Pts',(1.61565150075097,-1.84778273272244,2.14930655264067));
#9536=CARTESIAN_POINT('Ctrl Pts',(1.00523203996909,-2.38151708026416,2.1069831502227));
#9537=CARTESIAN_POINT('Ctrl Pts',(0.104194171581416,-2.58287794161623,2.06465974780474));
#9538=CARTESIAN_POINT('Ctrl Pts',(-0.675361720300282,-2.35977058887531,
2.02233634538678));
#9539=CARTESIAN_POINT('Ctrl Pts',(-1.45491761218198,-2.13666323613438,1.98001294296881));
#9540=CARTESIAN_POINT('Ctrl Pts',(-2.11299152755771,-1.48908766930046,1.93768954055085));
#9541=CARTESIAN_POINT('Ctrl Pts',(-2.34860550835862,-0.713220169978244,
1.89536613813289));
#9542=CARTESIAN_POINT('Ctrl Pts',(-2.4182645964874,-0.483835553972742,1.88285325749261));
#9543=CARTESIAN_POINT('Ctrl Pts',(-2.45099711338713,-0.243237138041082,
1.87034037685233));
#9544=CARTESIAN_POINT('Ctrl Pts',(-2.44901144034399,-0.00211142026644101,
1.85782749621206));
#9545=CARTESIAN_POINT('Ctrl Pts',(-2.44927322928455,-0.00216311090478056,
1.74217250378796));
#9546=CARTESIAN_POINT('Ctrl Pts',(-2.45124245034903,-0.233792226701819,
1.75419582883738));
#9547=CARTESIAN_POINT('Ctrl Pts',(-2.42106894900518,-0.464918469377862,
1.7662191538868));
#9548=CARTESIAN_POINT('Ctrl Pts',(-2.35668248545627,-0.686084490105454,
1.77824247893622));
#9549=CARTESIAN_POINT('Ctrl Pts',(-2.12995108334824,-1.46490163915,1.82058158557756));
#9550=CARTESIAN_POINT('Ctrl Pts',(-1.47896672116872,-2.12020847595462,1.8629206922189));
#9551=CARTESIAN_POINT('Ctrl Pts',(-0.701667462640163,-2.35208966279054,
1.90525979886024));
#9552=CARTESIAN_POINT('Ctrl Pts',(0.0756317958883954,-2.58397084962646,
1.94759890550158));
#9553=CARTESIAN_POINT('Ctrl Pts',(0.979245950765992,-2.39242638649367,1.98993801214292));
#9554=CARTESIAN_POINT('Ctrl Pts',(1.59561556779576,-1.86512056429426,2.03227711878426));
#9555=CARTESIAN_POINT('Ctrl Pts',(2.21198518482554,-1.33781474209484,2.07461622542559));
#9556=CARTESIAN_POINT('Ctrl Pts',(2.54111026400748,-0.474747560828786,2.11695533206693));
#9557=CARTESIAN_POINT('Ctrl Pts',(2.43235915396947,0.329078447597896,2.15929443870827));
#9558=CARTESIAN_POINT('Ctrl Pts',(2.32360804393145,1.13290445602459,2.20163354534961));
#9559=CARTESIAN_POINT('Ctrl Pts',(1.77698074467345,1.8774892916119,2.24397265199095));
#9560=CARTESIAN_POINT('Ctrl Pts',(1.04265371162473,2.22205687499011,2.28631175863229));
#9561=CARTESIAN_POINT('Ctrl Pts',(0.308326678576009,2.56662445836832,2.32865086527363));
#9562=CARTESIAN_POINT('Ctrl Pts',(-0.613700088263441,2.51117478953743,2.37098997191497));
#9563=CARTESIAN_POINT('Ctrl Pts',(-1.30144008604655,2.08108561434068,2.4133290785563));
#9564=CARTESIAN_POINT('Ctrl Pts',(-1.98918008382967,1.65099643914393,2.45566818519764));
#9565=CARTESIAN_POINT('Ctrl Pts',(-2.44263331255644,0.84626775758132,2.49800729183898));
#9566=CARTESIAN_POINT('Ctrl Pts',(-2.45426657710675,0.0352019852067503,
2.54034639848032));
#9567=CARTESIAN_POINT('Ctrl Pts',(-2.45443382647206,0.0235414375533725,
2.54095510024953));
#9568=CARTESIAN_POINT('Ctrl Pts',(-2.45450975474792,0.0118795800677466,
2.54156380201875));
#9569=CARTESIAN_POINT('Ctrl Pts',(-2.45449494699467,0.000217524429918226,
2.54217250378796));
#9570=CARTESIAN_POINT('Origin',(0.,0.,0.));
#9571=CARTESIAN_POINT('',(-2.44879028350035,0.00206176536797276,3.45782749621206));
#9572=CARTESIAN_POINT('',(-2.44863779808279,0.00202668083941567,3.34217250378796));
#9573=CARTESIAN_POINT('',(-2.4505,-3.00099698131059E-16,0.));
#9574=CARTESIAN_POINT('Ctrl Pts',(-2.44879028350035,0.00206176536797276,
3.45782749621206));
#9575=CARTESIAN_POINT('Ctrl Pts',(-2.4507822485306,0.25146786442212,3.44488787253455));
#9576=CARTESIAN_POINT('Ctrl Pts',(-2.41573172748871,0.500327341519915,3.43194824885704));
#9577=CARTESIAN_POINT('Ctrl Pts',(-2.34131554709139,0.736798669794325,3.41900862517953));
#9578=CARTESIAN_POINT('Ctrl Pts',(-2.09791233631349,1.51025788594317,3.37668522276156));
#9579=CARTESIAN_POINT('Ctrl Pts',(-1.43336050190279,2.15118402855148,3.3343618203436));
#9580=CARTESIAN_POINT('Ctrl Pts',(-0.651600735693898,2.36644189707647,3.29203841792564));
#9581=CARTESIAN_POINT('Ctrl Pts',(0.130159030514992,2.58169976560146,3.24971501550768));
#9582=CARTESIAN_POINT('Ctrl Pts',(1.02912672852208,2.37128936004313,3.20739161308971));
#9583=CARTESIAN_POINT('Ctrl Pts',(1.63414878100557,1.8314443841374,3.16506821067175));
#9584=CARTESIAN_POINT('Ctrl Pts',(2.23917083348905,1.29159940823166,3.12274480825379));
#9585=CARTESIAN_POINT('Ctrl Pts',(2.55024724044895,0.422319861978524,3.08042140583583));
#9586=CARTESIAN_POINT('Ctrl Pts',(2.42510350427122,-0.378818907200365,3.03809800341787));
#9587=CARTESIAN_POINT('Ctrl Pts',(2.2999597680935,-1.17995767637926,2.99577460099991));
#9588=CARTESIAN_POINT('Ctrl Pts',(1.73859588877812,-1.91295566848391,2.95345119858194));
#9589=CARTESIAN_POINT('Ctrl Pts',(0.99775831871812,-2.24256752609274,2.91112779616398));
#9590=CARTESIAN_POINT('Ctrl Pts',(0.256920748658124,-2.57217938370157,2.86880439374602));
#9591=CARTESIAN_POINT('Ctrl Pts',(-0.663390512146504,-2.4984051068146,2.82648099132806));
#9592=CARTESIAN_POINT('Ctrl Pts',(-1.34226015405468,-2.05498624035627,2.7841575889101));
#9593=CARTESIAN_POINT('Ctrl Pts',(-2.01770730537467,-1.61380285005329,2.74204755801075));
#9594=CARTESIAN_POINT('Ctrl Pts',(-2.45414113525188,-0.806692568145523,
2.6999375271114));
#9595=CARTESIAN_POINT('Ctrl Pts',(-2.45450932558232,7.6261763116035E-5,
2.65782749621206));
#9596=CARTESIAN_POINT('Ctrl Pts',(-2.45449494699467,0.000217524429918226,
2.54217250378796));
#9597=CARTESIAN_POINT('Ctrl Pts',(-2.45347978066934,-0.799291082283641,
2.58390290866009));
#9598=CARTESIAN_POINT('Ctrl Pts',(-2.02600703470396,-1.59973100051144,2.62563331353221));
#9599=CARTESIAN_POINT('Ctrl Pts',(-1.3605912120938,-2.04290360643243,2.66736371840434));
#9600=CARTESIAN_POINT('Ctrl Pts',(-0.685469282156714,-2.49254056251051,
2.70970282504568));
#9601=CARTESIAN_POINT('Ctrl Pts',(0.234587878091294,-2.57441161148015,2.75204193168701));
#9602=CARTESIAN_POINT('Ctrl Pts',(0.978495183990076,-2.25104659733286,2.79438103832835));
#9603=CARTESIAN_POINT('Ctrl Pts',(1.72240248988886,-1.92768158318556,2.83672014496969));
#9604=CARTESIAN_POINT('Ctrl Pts',(2.29015994143841,-1.19908050592133,2.87905925161103));
#9605=CARTESIAN_POINT('Ctrl Pts',(2.42192042487556,-0.398704226023195,2.92139835825237));
#9606=CARTESIAN_POINT('Ctrl Pts',(2.55368090831271,0.401672053874929,2.96373746489371));
#9607=CARTESIAN_POINT('Ctrl Pts',(2.24944442363746,1.27382353640695,3.00607657153505));
#9608=CARTESIAN_POINT('Ctrl Pts',(1.6484517191997,1.81859025937093,3.04841567817639));
#9609=CARTESIAN_POINT('Ctrl Pts',(1.04745901476194,2.36335698233492,3.09075478481772));
#9610=CARTESIAN_POINT('Ctrl Pts',(0.149710090561681,2.58073894573087,3.13309389145906));
#9611=CARTESIAN_POINT('Ctrl Pts',(-0.633919837933851,2.37124634813164,3.1754329981004));
#9612=CARTESIAN_POINT('Ctrl Pts',(-1.41754976642938,2.16175375053241,3.21777210474174));
#9613=CARTESIAN_POINT('Ctrl Pts',(-2.08706069922018,1.525386591938,3.26011121138308));
#9614=CARTESIAN_POINT('Ctrl Pts',(-2.33603572860561,0.75339277828086,3.30245031802442));
#9615=CARTESIAN_POINT('Ctrl Pts',(-2.41389780579042,0.511966792496097,3.31569104661227));
#9616=CARTESIAN_POINT('Ctrl Pts',(-2.4506313265692,0.257276473065291,3.32893177520011));
#9617=CARTESIAN_POINT('Ctrl Pts',(-2.44863779808279,0.00202668083941567,
3.34217250378796));
#9618=CARTESIAN_POINT('Origin',(0.,0.,0.));
#9619=CARTESIAN_POINT('',(-2.44722122097757,-0.00133409068037049,4.25782749621205));
#9620=CARTESIAN_POINT('',(-2.44727990084847,-0.00138675037849539,4.14217250378796));
#9621=CARTESIAN_POINT('',(-2.4505,-3.00099698131059E-16,0.));
#9622=CARTESIAN_POINT('Ctrl Pts',(-2.44722122097757,-0.00133409068037049,
4.25782749621205));
#9623=CARTESIAN_POINT('Ctrl Pts',(-2.44476959024658,0.494163923095195,4.23216162037565));
#9624=CARTESIAN_POINT('Ctrl Pts',(-2.29877320492706,0.990990135522418,4.20649574453925));
#9625=CARTESIAN_POINT('Ctrl Pts',(-2.01920729690624,1.39550444749988,4.18082986870284));
#9626=CARTESIAN_POINT('Ctrl Pts',(-1.55819904988879,2.06255442930348,4.13850646628488));
#9627=CARTESIAN_POINT('Ctrl Pts',(-0.733982018406264,2.47858537266224,4.09618306386692));
#9628=CARTESIAN_POINT('Ctrl Pts',(0.0764783273015039,2.4533205734938,4.05385966144895));
#9629=CARTESIAN_POINT('Ctrl Pts',(0.886938673009272,2.42805577432537,4.01153625903099));
#9630=CARTESIAN_POINT('Ctrl Pts',(1.68364233294229,1.96149523262974,3.96921285661303));
#9631=CARTESIAN_POINT('Ctrl Pts',(2.10220740483942,1.26702596575867,3.92688945419507));
#9632=CARTESIAN_POINT('Ctrl Pts',(2.52077247673655,0.572556698887595,3.88456605177711));
#9633=CARTESIAN_POINT('Ctrl Pts',(2.5611989605978,-0.349821293158926,3.84224264935915));
#9634=CARTESIAN_POINT('Ctrl Pts',(2.20499732281998,-1.07824745639663,3.79991924694118));
#9635=CARTESIAN_POINT('Ctrl Pts',(1.84879568504216,-1.80667361963432,3.75759584452322));
#9636=CARTESIAN_POINT('Ctrl Pts',(1.09596592562527,-2.3411479540632,3.71527244210526));
#9637=CARTESIAN_POINT('Ctrl Pts',(0.290823696188848,-2.43722226081783,3.67294903968729));
#9638=CARTESIAN_POINT('Ctrl Pts',(-0.514318533247575,-2.53329656757247,
3.63062563726933));
#9639=CARTESIAN_POINT('Ctrl Pts',(-1.37177323270354,-2.19097084665287,3.58830223485137));
#9640=CARTESIAN_POINT('Ctrl Pts',(-1.88937328885896,-1.56681184134837,3.54597883243341));
#9641=CARTESIAN_POINT('Ctrl Pts',(-2.24872638093603,-1.13347829387951,3.51659505369296));
#9642=CARTESIAN_POINT('Ctrl Pts',(-2.44426685521786,-0.564298881106139,
3.48721127495251));
#9643=CARTESIAN_POINT('Ctrl Pts',(-2.44879028350035,0.00206176536797276,
3.45782749621206));
#9644=CARTESIAN_POINT('Ctrl Pts',(-2.44863779808279,0.00202668083941567,
3.34217250378796));
#9645=CARTESIAN_POINT('Ctrl Pts',(-2.44425673663492,-0.558920921325063,
3.37127088184145));
#9646=CARTESIAN_POINT('Ctrl Pts',(-2.25283838345664,-1.12257056969168,3.40036925989494));
#9647=CARTESIAN_POINT('Ctrl Pts',(-1.89987184308078,-1.55407547542566,3.42946763794843));
#9648=CARTESIAN_POINT('Ctrl Pts',(-1.38629380219047,-2.18192944675517,3.47180674458977));
#9649=CARTESIAN_POINT('Ctrl Pts',(-0.530698594429779,-2.5300169206943,3.51414585123111));
#9650=CARTESIAN_POINT('Ctrl Pts',(0.275331171558287,-2.43902774682149,3.55648495787245));
#9651=CARTESIAN_POINT('Ctrl Pts',(1.08136093754636,-2.34803857294868,3.59882406451379));
#9652=CARTESIAN_POINT('Ctrl Pts',(1.8378252617618,-1.81797275126393,3.64116317115513));
#9653=CARTESIAN_POINT('Ctrl Pts',(2.19851103921323,-1.09142696233993,3.68350227779647));
#9654=CARTESIAN_POINT('Ctrl Pts',(2.55919681666466,-0.364881173415942,3.72584138443781));
#9655=CARTESIAN_POINT('Ctrl Pts',(2.52410404735208,0.558144582747287,3.76818049107915));
#9656=CARTESIAN_POINT('Ctrl Pts',(2.10929373540885,1.25520657320205,3.81051959772049));
#9657=CARTESIAN_POINT('Ctrl Pts',(1.69448342346561,1.95226856365681,3.85285870436182));
#9658=CARTESIAN_POINT('Ctrl Pts',(0.899955568891718,2.42336678840311,3.89519781100316));
#9659=CARTESIAN_POINT('Ctrl Pts',(0.0893439171220223,2.45289242898376,3.9375369176445));
#9660=CARTESIAN_POINT('Ctrl Pts',(-0.721267734647671,2.48241806956442,3.97987602428584));
#9661=CARTESIAN_POINT('Ctrl Pts',(-1.54796318361316,2.07037112597943,4.02221513092718));
#9662=CARTESIAN_POINT('Ctrl Pts',(-2.0123864530499,1.40533425463558,4.06455423756852));
#9663=CARTESIAN_POINT('Ctrl Pts',(-2.29618813448365,0.998940788322545,4.090426992975));
#9664=CARTESIAN_POINT('Ctrl Pts',(-2.44470876469706,0.498074863705097,4.11629974838148));
#9665=CARTESIAN_POINT('Ctrl Pts',(-2.44727990084847,-0.00138675037849539,
4.14217250378796));
#9666=CARTESIAN_POINT('Origin',(0.,0.,0.));
#9667=CARTESIAN_POINT('',(-2.45364436265411,-0.00130297157212494,5.05782749621206));
#9668=CARTESIAN_POINT('',(-2.45368883860995,-0.00127745634613248,4.94217250378796));
#9669=CARTESIAN_POINT('',(-2.4505,-3.00099698131059E-16,0.));
#9670=CARTESIAN_POINT('Ctrl Pts',(-2.45364436265411,-0.00130297157212494,
5.05782749621206));
#9671=CARTESIAN_POINT('Ctrl Pts',(-2.44890065072277,0.734926114472917,5.01943536821676));
#9672=CARTESIAN_POINT('Ctrl Pts',(-2.09516161037558,1.47510769560909,4.98104324022146));
#9673=CARTESIAN_POINT('Ctrl Pts',(-1.51690197902683,1.92967332906283,4.94265111222616));
#9674=CARTESIAN_POINT('Ctrl Pts',(-0.879429758611428,2.43078554228515,4.9003277098082));
#9675=CARTESIAN_POINT('Ctrl Pts',(0.0308981140190441,2.58479406519437,4.85800430739023));
#9676=CARTESIAN_POINT('Ctrl Pts',(0.797732350424128,2.32126126663045,4.81568090497227));
#9677=CARTESIAN_POINT('Ctrl Pts',(1.56456658682921,2.05772846806654,4.77335750255431));
#9678=CARTESIAN_POINT('Ctrl Pts',(2.18790718700891,1.37665434802948,4.73103410013635));
#9679=CARTESIAN_POINT('Ctrl Pts',(2.38266190766968,0.589536262338264,4.68871069771839));
#9680=CARTESIAN_POINT('Ctrl Pts',(2.57741662833046,-0.197581823352954,4.64638729530042));
#9681=CARTESIAN_POINT('Ctrl Pts',(2.34358546947232,-1.09074387469833,4.60406389288246));
#9682=CARTESIAN_POINT('Ctrl Pts',(1.78811389495814,-1.68145159595198,4.5617404904645));
#9683=CARTESIAN_POINT('Ctrl Pts',(1.23264232044396,-2.27215931720563,4.51941708804654));
#9684=CARTESIAN_POINT('Ctrl Pts',(0.355530330273727,-2.56041270836756,4.47709368562858));
#9685=CARTESIAN_POINT('Ctrl Pts',(-0.442064466333378,-2.41437564982704,
4.43477028321061));
#9686=CARTESIAN_POINT('Ctrl Pts',(-1.23965926294048,-2.26833859128653,4.39244688079265));
#9687=CARTESIAN_POINT('Ctrl Pts',(-1.95773686598445,-1.68801108304359,4.35012347837469));
#9688=CARTESIAN_POINT('Ctrl Pts',(-2.26787593623026,-0.938812818797895,
4.30780007595673));
#9689=CARTESIAN_POINT('Ctrl Pts',(-2.38993960577132,-0.643945457277985,
4.29114254937517));
#9690=CARTESIAN_POINT('Ctrl Pts',(-2.44881236496696,-0.322919505812342,
4.27448502279361));
#9691=CARTESIAN_POINT('Ctrl Pts',(-2.44722122097757,-0.00133409068037049,
4.25782749621205));
#9692=CARTESIAN_POINT('Ctrl Pts',(-2.44727990084847,-0.00138675037849539,
4.14217250378796));
#9693=CARTESIAN_POINT('Ctrl Pts',(-2.4489162642847,-0.319262068898655,4.15863885502282));
#9694=CARTESIAN_POINT('Ctrl Pts',(-2.39143568339083,-0.636568570457953,
4.17510520625768));
#9695=CARTESIAN_POINT('Ctrl Pts',(-2.27208795289109,-0.928590296092531,
4.19157155749253));
#9696=CARTESIAN_POINT('Ctrl Pts',(-1.96521509338757,-1.67945117637405,4.23391066413387));
#9697=CARTESIAN_POINT('Ctrl Pts',(-1.24931828447256,-2.2631461378344,4.27624977077521));
#9698=CARTESIAN_POINT('Ctrl Pts',(-0.452043984954612,-2.41253390428878,
4.31858887741655));
#9699=CARTESIAN_POINT('Ctrl Pts',(0.345230314563356,-2.56192167074316,4.36092798405789));
#9700=CARTESIAN_POINT('Ctrl Pts',(1.22388210468428,-2.27700224219155,4.40326709069923));
#9701=CARTESIAN_POINT('Ctrl Pts',(1.78177640732824,-1.68817547605737,4.44560619734057));
#9702=CARTESIAN_POINT('Ctrl Pts',(2.33967070997219,-1.09934870992319,4.4879453039819));
#9703=CARTESIAN_POINT('Ctrl Pts',(2.5768075251392,-0.206614606206465,4.53028441062324));
#9704=CARTESIAN_POINT('Ctrl Pts',(2.38465579531495,0.581446765872876,4.57262351726458));
#9705=CARTESIAN_POINT('Ctrl Pts',(2.19250406549071,1.36950813795221,4.61496262390592));
#9706=CARTESIAN_POINT('Ctrl Pts',(1.57106379067523,2.05289677839415,4.65730173054726));
#9707=CARTESIAN_POINT('Ctrl Pts',(0.804751248283616,2.31884433113998,4.6996408371886));
#9708=CARTESIAN_POINT('Ctrl Pts',(0.0384387058919862,2.58479188388582,4.74197994382993));
#9709=CARTESIAN_POINT('Ctrl Pts',(-0.872746104075775,2.43329834893554,4.78431905047128));
#9710=CARTESIAN_POINT('Ctrl Pts',(-1.51177872699224,1.93369818852045,4.82665815711262));
#9711=CARTESIAN_POINT('Ctrl Pts',(-2.09293912294914,1.4793429386713,4.86516293933773));
#9712=CARTESIAN_POINT('Ctrl Pts',(-2.44900869472268,0.737076692851381,4.90366772156284));
#9713=CARTESIAN_POINT('Ctrl Pts',(-2.45368883860995,-0.00127745634613248,
4.94217250378796));
#9714=CARTESIAN_POINT('Origin',(0.,0.,0.));
#9715=CARTESIAN_POINT('',(-2.45111861015583,0.00218804967254627,5.85782749621206));
#9716=CARTESIAN_POINT('',(-2.45112004158473,0.00219228095941415,5.74217250378796));
#9717=CARTESIAN_POINT('',(-2.4505,-3.00099698131059E-16,0.));
#9718=CARTESIAN_POINT('Ctrl Pts',(-2.45111861015583,0.00218804967254627,
5.85782749621206));
#9719=CARTESIAN_POINT('Ctrl Pts',(-2.45267722565121,0.171297744836882,5.84903251847582));
#9720=CARTESIAN_POINT('Ctrl Pts',(-2.43666676456879,0.340114246849872,5.84023754073959));
#9721=CARTESIAN_POINT('Ctrl Pts',(-2.40199867071989,0.505008075907527,5.83144256300336));
#9722=CARTESIAN_POINT('Ctrl Pts',(-2.23516803953071,1.29851410773017,5.7891191605854));
#9723=CARTESIAN_POINT('Ctrl Pts',(-1.63627329148971,2.00118084351996,5.74679575816743));
#9724=CARTESIAN_POINT('Ctrl Pts',(-0.879226068428833,2.29163528762042,5.70447235574947));
#9725=CARTESIAN_POINT('Ctrl Pts',(-0.122178845367954,2.58208973172088,5.66214895333151));
#9726=CARTESIAN_POINT('Ctrl Pts',(0.793020852712802,2.460331884132,5.61982555091355));
#9727=CARTESIAN_POINT('Ctrl Pts',(1.44779555001256,1.98204914576702,5.57750214849559));
#9728=CARTESIAN_POINT('Ctrl Pts',(2.10257024731232,1.50376640740205,5.53517874607763));
#9729=CARTESIAN_POINT('Ctrl Pts',(2.49691994383109,0.668958778260969,5.49285534365967));
#9730=CARTESIAN_POINT('Ctrl Pts',(2.45048411180883,-0.140564535514672,5.4505319412417));
#9731=CARTESIAN_POINT('Ctrl Pts',(2.40404827978657,-0.950087849290307,5.40820853882374));
#9732=CARTESIAN_POINT('Ctrl Pts',(1.91682691922329,-1.73432684770051,5.36588513640578));
#9733=CARTESIAN_POINT('Ctrl Pts',(1.21165651890775,-2.13460048980139,5.32356173398782));
#9734=CARTESIAN_POINT('Ctrl Pts',(0.506486118592195,-2.53487413190227,5.28123833156986));
#9735=CARTESIAN_POINT('Ctrl Pts',(-0.416633321475635,-2.55118241769382,
5.23891492915189));
#9736=CARTESIAN_POINT('Ctrl Pts',(-1.13550213722612,-2.17606655854707,5.19659152673393));
#9737=CARTESIAN_POINT('Ctrl Pts',(-1.8543709529766,-1.80095069940033,5.15426812431597));
#9738=CARTESIAN_POINT('Ctrl Pts',(-2.36898914440973,-1.03441069531529,5.11194472189801));
#9739=CARTESIAN_POINT('Ctrl Pts',(-2.44398995602614,-0.227032741505079,
5.06962131948004));
#9740=CARTESIAN_POINT('Ctrl Pts',(-2.45095652193392,-0.152038196692948,
5.06569004505738));
#9741=CARTESIAN_POINT('Ctrl Pts',(-2.45413010893487,-0.0766913057520759,
5.06175877063472));
#9742=CARTESIAN_POINT('Ctrl Pts',(-2.45364436265411,-0.00130297157212494,
5.05782749621206));
#9743=CARTESIAN_POINT('Ctrl Pts',(-2.45368883860995,-0.00127745634613248,
4.94217250378796));
#9744=CARTESIAN_POINT('Ctrl Pts',(-2.45415488955067,-0.0748031115631014,
4.94600682820418));
#9745=CARTESIAN_POINT('Ctrl Pts',(-2.45113646785659,-0.14828997337155,4.94984115262041));
#9746=CARTESIAN_POINT('Ctrl Pts',(-2.4445088578359,-0.221449876124288,4.95367547703663));
#9747=CARTESIAN_POINT('Ctrl Pts',(-2.37132592989794,-1.02929099447407,4.99601458367797));
#9748=CARTESIAN_POINT('Ctrl Pts',(-1.85807963815686,-1.79726644529373,5.03835369031931));
#9749=CARTESIAN_POINT('Ctrl Pts',(-1.13966882262996,-2.1738947946943,5.08069279696065));
#9750=CARTESIAN_POINT('Ctrl Pts',(-0.421258007103072,-2.55052314409486,
5.12303190360199));
#9751=CARTESIAN_POINT('Ctrl Pts',(0.502317332209637,-2.53580439207634,5.16537101024333));
#9752=CARTESIAN_POINT('Ctrl Pts',(1.20836193308383,-2.13647491030144,5.20771011688466));
#9753=CARTESIAN_POINT('Ctrl Pts',(1.91440653395803,-1.73714542852654,5.250049223526));
#9754=CARTESIAN_POINT('Ctrl Pts',(2.40292039639372,-0.953205216995241,5.29238833016734));
#9755=CARTESIAN_POINT('Ctrl Pts',(2.45032403922356,-0.14344234547996,5.33472743680868));
#9756=CARTESIAN_POINT('Ctrl Pts',(2.4977276820534,0.666320526035315,5.37706654345001));
#9757=CARTESIAN_POINT('Ctrl Pts',(2.10402110527741,1.50190605753458,5.41940565009136));
#9758=CARTESIAN_POINT('Ctrl Pts',(1.44939307923848,1.98088952380724,5.4617447567327));
#9759=CARTESIAN_POINT('Ctrl Pts',(0.794765053199531,2.4598729900799,5.50408386337404));
#9760=CARTESIAN_POINT('Ctrl Pts',(-0.120784422102356,2.58225439112595,5.54642297001537));
#9761=CARTESIAN_POINT('Ctrl Pts',(-0.878233303668452,2.29202309499735,5.58876207665671));
#9762=CARTESIAN_POINT('Ctrl Pts',(-1.63568218523454,2.00179179886876,5.63110118329805));
#9763=CARTESIAN_POINT('Ctrl Pts',(-2.23503047306484,1.2989478055655,5.67344028993939));
#9764=CARTESIAN_POINT('Ctrl Pts',(-2.40197279010514,0.505163655925678,5.71577939658073));
#9765=CARTESIAN_POINT('Ctrl Pts',(-2.43666196850777,0.34022213319964,5.72457709898314));
#9766=CARTESIAN_POINT('Ctrl Pts',(-2.45268103865343,0.17135406301958,5.73337480138555));
#9767=CARTESIAN_POINT('Ctrl Pts',(-2.45112004158473,0.00219228095941415,
5.74217250378796));
#9768=CARTESIAN_POINT('Origin',(0.,0.,0.));
#9769=CARTESIAN_POINT('',(-2.44649108011119,-0.000113800941714537,6.65782749621206));
#9770=CARTESIAN_POINT('',(-2.44648217412756,-8.24998363560429E-5,6.54217250378796));
#9771=CARTESIAN_POINT('',(-2.4505,-3.00099698131059E-16,0.));
#9772=CARTESIAN_POINT('Ctrl Pts',(-2.44649108011119,-0.000113800941714537,
6.65782749621206));
#9773=CARTESIAN_POINT('Ctrl Pts',(-2.44631871903483,0.415678882547852,6.63630626631693));
#9774=CARTESIAN_POINT('Ctrl Pts',(-2.34588140389044,0.831549710158929,6.6147850364218));
#9775=CARTESIAN_POINT('Ctrl Pts',(-2.14564944517726,1.19198122018866,6.59326380652668));
#9776=CARTESIAN_POINT('Ctrl Pts',(-1.75187558527936,1.90080166945843,6.55094040410871));
#9777=CARTESIAN_POINT('Ctrl Pts',(-0.972148917036941,2.39521221106142,6.50861700169075));
#9778=CARTESIAN_POINT('Ctrl Pts',(-0.163086713480121,2.4490882986855,6.46629359927279));
#9779=CARTESIAN_POINT('Ctrl Pts',(0.645975490076699,2.50296438630957,6.42397019685483));
#9780=CARTESIAN_POINT('Ctrl Pts',(1.48437322894793,2.11630601995472,6.38164679443687));
#9781=CARTESIAN_POINT('Ctrl Pts',(1.96865531757284,1.4659560059784,6.33932339201891));
#9782=CARTESIAN_POINT('Ctrl Pts',(2.45293740619775,0.815605992002093,6.29699998960095));
#9783=CARTESIAN_POINT('Ctrl Pts',(2.58310384457635,-0.0984356695956784,
6.25467658718298));
#9784=CARTESIAN_POINT('Ctrl Pts',(2.29962146270785,-0.85812114478397,6.21235318476502));
#9785=CARTESIAN_POINT('Ctrl Pts',(2.01613908083936,-1.61780661997226,6.17002978234706));
#9786=CARTESIAN_POINT('Ctrl Pts',(1.31900787872379,-2.22313590875106,6.12770637992909));
#9787=CARTESIAN_POINT('Ctrl Pts',(0.527069109800669,-2.39725445548984,6.08538297751113));
#9788=CARTESIAN_POINT('Ctrl Pts',(-0.264869659122454,-2.57137300222862,
6.04305957509317));
#9789=CARTESIAN_POINT('Ctrl Pts',(-1.15161599485312,-2.31428080692735,6.00073617267521));
#9790=CARTESIAN_POINT('Ctrl Pts',(-1.72760590554977,-1.74356204534898,5.95841277025725));
#9791=CARTESIAN_POINT('Ctrl Pts',(-2.18390273507956,-1.29144099839104,5.92488434557552));
#9792=CARTESIAN_POINT('Ctrl Pts',(-2.4451768188504,-0.642495978794029,5.89135592089379));
#9793=CARTESIAN_POINT('Ctrl Pts',(-2.45111861015583,0.00218804967254627,
5.85782749621206));
#9794=CARTESIAN_POINT('Ctrl Pts',(-2.45112004158473,0.00219228095941415,
5.74217250378796));
#9795=CARTESIAN_POINT('Ctrl Pts',(-2.44516871119164,-0.642740163254894,
5.77571390802689));
#9796=CARTESIAN_POINT('Ctrl Pts',(-2.18368586072072,-1.29194179724376,5.80925531226582));
#9797=CARTESIAN_POINT('Ctrl Pts',(-1.727077308387,-1.74409505891404,5.84279671650475));
#9798=CARTESIAN_POINT('Ctrl Pts',(-1.15070316337826,-2.31484531813751,5.88513582314608));
#9799=CARTESIAN_POINT('Ctrl Pts',(-0.263418527110475,-2.57162153060804,
5.92747492978742));
#9800=CARTESIAN_POINT('Ctrl Pts',(0.528690603930214,-2.39690422190574,5.96981403642876));
#9801=CARTESIAN_POINT('Ctrl Pts',(1.3207997349709,-2.22218691320345,6.0121531430701));
#9802=CARTESIAN_POINT('Ctrl Pts',(2.0177333607845,-1.61597608332832,6.05449224971144));
#9803=CARTESIAN_POINT('Ctrl Pts',(2.30052395465526,-0.855717907800806,6.09683135635278));
#9804=CARTESIAN_POINT('Ctrl Pts',(2.58331454852602,-0.0954597322732809,
6.13917046299412));
#9805=CARTESIAN_POINT('Ctrl Pts',(2.45196211045394,0.818845788906634,6.18150956963546));
#9806=CARTESIAN_POINT('Ctrl Pts',(1.96658307154252,1.46874593663984,6.22384867627679));
#9807=CARTESIAN_POINT('Ctrl Pts',(1.48120403263111,2.11864608437304,6.26618778291813));
#9808=CARTESIAN_POINT('Ctrl Pts',(0.641798392880346,2.50414085865953,6.30852688955947));
#9809=CARTESIAN_POINT('Ctrl Pts',(-0.167460763063443,2.44879980735622,6.35086599620081));
#9810=CARTESIAN_POINT('Ctrl Pts',(-0.976719919007238,2.39345875605291,6.39320510284215));
#9811=CARTESIAN_POINT('Ctrl Pts',(-1.75583259114405,1.89728187915982,6.43554420948349));
#9812=CARTESIAN_POINT('Ctrl Pts',(-2.14822014291542,1.18735581071813,6.47788331612483));
#9813=CARTESIAN_POINT('Ctrl Pts',(-2.34682515967691,0.828030245761283,6.49931304534587));
#9814=CARTESIAN_POINT('Ctrl Pts',(-2.44635784802019,0.413945812065253,6.52074277456692));
#9815=CARTESIAN_POINT('Ctrl Pts',(-2.44648217412756,-8.24998363560429E-5,
6.54217250378796));
#9816=CARTESIAN_POINT('Origin',(0.,0.,0.));
#9817=CARTESIAN_POINT('',(-2.45153584345453,-0.0021256739944922,7.45782749621206));
#9818=CARTESIAN_POINT('',(-2.45142289816278,-0.00214958505015697,7.34217250378796));
#9819=CARTESIAN_POINT('',(-2.4505,-3.00099698131059E-16,0.));
#9820=CARTESIAN_POINT('Ctrl Pts',(-2.45153584345453,-0.00212567399449221,
7.45782749621206));
#9821=CARTESIAN_POINT('Ctrl Pts',(-2.44552947185313,0.656095934058606,7.42358001415804));
#9822=CARTESIAN_POINT('Ctrl Pts',(-2.17165895316412,1.31872531414478,7.38933253210402));
#9823=CARTESIAN_POINT('Ctrl Pts',(-1.69781926623356,1.77258018438606,7.35508505005));
#9824=CARTESIAN_POINT('Ctrl Pts',(-1.11224314358814,2.33345885810207,7.31276164763203));
#9825=CARTESIAN_POINT('Ctrl Pts',(-0.221268524773137,2.57549127213791,7.27043824521407));
#9826=CARTESIAN_POINT('Ctrl Pts',(0.567606742770822,2.38798102095328,7.2281148427961));
#9827=CARTESIAN_POINT('Ctrl Pts',(1.35648201031479,2.20047076976864,7.18579144037814));
#9828=CARTESIAN_POINT('Ctrl Pts',(2.04325792658772,1.58341785336352,7.14346803796019));
#9829=CARTESIAN_POINT('Ctrl Pts',(2.31382935139211,0.81903876801305,7.10114463554222));
#9830=CARTESIAN_POINT('Ctrl Pts',(2.5844007761965,0.0546596826625877,7.05882123312426));
#9831=CARTESIAN_POINT('Ctrl Pts',(2.43876770953236,-0.857045571633228,7.0164978307063));
#9832=CARTESIAN_POINT('Ctrl Pts',(1.94353716795057,-1.49909774453391,6.97417442828833));
#9833=CARTESIAN_POINT('Ctrl Pts',(1.44830662636876,-2.1411499174346,6.93185102587037));
#9834=CARTESIAN_POINT('Ctrl Pts',(0.603478609869307,-2.51354900894016,6.88952762345241));
#9835=CARTESIAN_POINT('Ctrl Pts',(-0.204554731972394,-2.44597386177769,
6.84720422103445));
#9836=CARTESIAN_POINT('Ctrl Pts',(-1.0125880738141,-2.37839871461522,6.80488081861649));
#9837=CARTESIAN_POINT('Ctrl Pts',(-1.78382674099803,-1.87084932878471,6.76255741619853));
#9838=CARTESIAN_POINT('Ctrl Pts',(-2.1655355488133,-1.15545945740118,6.72023401378057));
#9839=CARTESIAN_POINT('Ctrl Pts',(-2.35314741411761,-0.803841613007534,
6.69943184125773));
#9840=CARTESIAN_POINT('Ctrl Pts',(-2.44665768233904,-0.402014211737506,
6.6786296687349));
#9841=CARTESIAN_POINT('Ctrl Pts',(-2.44649108011119,-0.000113800941714537,
6.65782749621206));
#9842=CARTESIAN_POINT('Ctrl Pts',(-2.44648217412756,-8.24998363560429E-5,
6.54217250378796));
#9843=CARTESIAN_POINT('Ctrl Pts',(-2.44660348137673,-0.404057470632325,
6.56308188120826));
#9844=CARTESIAN_POINT('Ctrl Pts',(-2.35208543716669,-0.807979012017471,
6.58399125862855));
#9845=CARTESIAN_POINT('Ctrl Pts',(-2.16261589659925,-1.16092897605749,6.60490063604884));
#9846=CARTESIAN_POINT('Ctrl Pts',(-1.77896166710579,-1.87561243440111,6.64723974269018));
#9847=CARTESIAN_POINT('Ctrl Pts',(-1.00599077671297,-2.38130409109805,6.68957884933152));
#9848=CARTESIAN_POINT('Ctrl Pts',(-0.19747093585954,-2.44656265670112,6.73191795597286));
#9849=CARTESIAN_POINT('Ctrl Pts',(0.611048904993884,-2.51182122230418,6.7742570626142));
#9850=CARTESIAN_POINT('Ctrl Pts',(1.45511769630792,-2.13664669681336,6.81659616925554));
#9851=CARTESIAN_POINT('Ctrl Pts',(1.94842815605251,-1.49274623575995,6.85893527589687));
#9852=CARTESIAN_POINT('Ctrl Pts',(2.44173861579709,-0.848845774706545,6.90127438253821));
#9853=CARTESIAN_POINT('Ctrl Pts',(2.58429074397226,0.0637806219094324,6.94361348917955));
#9854=CARTESIAN_POINT('Ctrl Pts',(2.3108423165441,0.827448724539928,6.98595259582089));
#9855=CARTESIAN_POINT('Ctrl Pts',(2.03739388911593,1.59111682717045,7.02829170246223));
#9856=CARTESIAN_POINT('Ctrl Pts',(1.34794490608442,2.20582663581546,7.07063080910357));
#9857=CARTESIAN_POINT('Ctrl Pts',(0.558037377145987,2.39024222399774,7.11296991574491));
#9858=CARTESIAN_POINT('Ctrl Pts',(-0.231870151792425,2.57465781218002,7.15530902238624));
#9859=CARTESIAN_POINT('Ctrl Pts',(-1.12223622663775,2.32877917989957,7.19764812902759));
#9860=CARTESIAN_POINT('Ctrl Pts',(-1.70556456044661,1.76513827611953,7.23998723566892));
#9861=CARTESIAN_POINT('Ctrl Pts',(-2.17485144374213,1.31168990458975,7.2740489917086));
#9862=CARTESIAN_POINT('Ctrl Pts',(-2.44541792823371,0.652580023487596,7.30811074774828));
#9863=CARTESIAN_POINT('Ctrl Pts',(-2.45142289816278,-0.00214958505015697,
7.34217250378796));
#9864=CARTESIAN_POINT('Origin',(0.,0.,0.));
#9865=CARTESIAN_POINT('',(-2.45333810822071,0.00149720406526131,8.25782749621206));
#9866=CARTESIAN_POINT('',(-2.45347385627323,0.00142195494216932,8.14217250378797));
#9867=CARTESIAN_POINT('',(-2.4505,-3.00099698131059E-16,0.));
#9868=CARTESIAN_POINT('Ctrl Pts',(-2.45333810822071,0.00149720406526131,
8.25782749621206));
#9869=CARTESIAN_POINT('Ctrl Pts',(-2.45397968238504,0.0907038896081416,
8.2531771644171));
#9870=CARTESIAN_POINT('Ctrl Pts',(-2.44953543463151,0.179845985026688,8.24852683262215));
#9871=CARTESIAN_POINT('Ctrl Pts',(-2.4397929040988,0.268405208558051,8.24387650082719));
#9872=CARTESIAN_POINT('Ctrl Pts',(-2.35112459859154,1.0743966561804,8.20155309840923));
#9873=CARTESIAN_POINT('Ctrl Pts',(-1.82359386603104,1.83210820223256,8.15922969599128));
#9874=CARTESIAN_POINT('Ctrl Pts',(-1.09847316630295,2.19499145187045,8.11690629357332));
#9875=CARTESIAN_POINT('Ctrl Pts',(-0.373352466574871,2.55787470150833,8.07458289115535));
#9876=CARTESIAN_POINT('Ctrl Pts',(0.549358200320791,2.52592965473193,8.03225948873738));
#9877=CARTESIAN_POINT('Ctrl Pts',(1.24764612759045,2.11376675893546,7.98993608631942));
#9878=CARTESIAN_POINT('Ctrl Pts',(1.94593405486012,1.70160386313898,7.94761268390145));
#9879=CARTESIAN_POINT('Ctrl Pts',(2.41979924250378,0.909223118322442,7.9052892814835));
#9880=CARTESIAN_POINT('Ctrl Pts',(2.45251380639982,0.0990292900622,7.86296587906554));
#9881=CARTESIAN_POINT('Ctrl Pts',(2.48522837029586,-0.711164538198042,7.82064247664758));
#9882=CARTESIAN_POINT('Ctrl Pts',(2.07679231044428,-1.53917144990198,7.77831907422961));
#9883=CARTESIAN_POINT('Ctrl Pts',(1.41400872054937,-2.00629262797885,7.73599567181165));
#9884=CARTESIAN_POINT('Ctrl Pts',(0.751225130654471,-2.47341380605572,7.69367226939369));
#9885=CARTESIAN_POINT('Ctrl Pts',(-0.165905989283751,-2.57964925050551,
7.65134886697573));
#9886=CARTESIAN_POINT('Ctrl Pts',(-0.917923804687642,-2.27641091625825,
7.60902546455777));
#9887=CARTESIAN_POINT('Ctrl Pts',(-1.66994162009153,-1.97317258201099,7.5667020621398));
#9888=CARTESIAN_POINT('Ctrl Pts',(-2.2568461309611,-1.26046046906668,7.52437865972183));
#9889=CARTESIAN_POINT('Ctrl Pts',(-2.41020957315796,-0.46424194589642,7.48205525730387));
#9890=CARTESIAN_POINT('Ctrl Pts',(-2.43947354711001,-0.312311878414712,
7.47397933693994));
#9891=CARTESIAN_POINT('Ctrl Pts',(-2.45295220973374,-0.157341326931424,
7.465903416576));
#9892=CARTESIAN_POINT('Ctrl Pts',(-2.45153584345453,-0.00212567399449221,
7.45782749621206));
#9893=CARTESIAN_POINT('Ctrl Pts',(-2.45142289816278,-0.00214958505015697,
7.34217250378796));
#9894=CARTESIAN_POINT('Ctrl Pts',(-2.45288216648111,-0.161255490008206,
7.35044985438962));
#9895=CARTESIAN_POINT('Ctrl Pts',(-2.43871804379984,-0.320102722758881,
7.35872720499128));
#9896=CARTESIAN_POINT('Ctrl Pts',(-2.40798566431321,-0.475677037637661,
7.36700455559294));
#9897=CARTESIAN_POINT('Ctrl Pts',(-2.25078784159854,-1.27144827233516,7.40934366223428));
#9898=CARTESIAN_POINT('Ctrl Pts',(-1.6601016033968,-1.98158756645051,7.45168276887562));
#9899=CARTESIAN_POINT('Ctrl Pts',(-0.9062679427176,-2.28108351878577,7.49402187551696));
#9900=CARTESIAN_POINT('Ctrl Pts',(-0.152434282038396,-2.58057947112103,
7.53636098215829));
#9901=CARTESIAN_POINT('Ctrl Pts',(0.76454680111826,-2.46943208167621,7.57870008879963));
#9902=CARTESIAN_POINT('Ctrl Pts',(1.42499805585471,-1.99851048145462,7.62103919544097));
#9903=CARTESIAN_POINT('Ctrl Pts',(2.08544931059115,-1.52758888123302,7.66337830208231));
#9904=CARTESIAN_POINT('Ctrl Pts',(2.48937073690738,-0.696893070234654,7.70571740872365));
#9905=CARTESIAN_POINT('Ctrl Pts',(2.45189850621544,0.113390118141594,7.74805651536499));
#9906=CARTESIAN_POINT('Ctrl Pts',(2.4144262755235,0.923673306517865,7.79039562200633));
#9907=CARTESIAN_POINT('Ctrl Pts',(1.93556038782336,1.71354387227202,7.83273472864767));
#9908=CARTESIAN_POINT('Ctrl Pts',(1.23446470918613,2.1214995841262,7.87507383528901));
#9909=CARTESIAN_POINT('Ctrl Pts',(0.533369030548933,2.52945529598037,7.91741294193035));
#9910=CARTESIAN_POINT('Ctrl Pts',(-0.389956439025329,2.5554961539346,7.95975204857168));
#9911=CARTESIAN_POINT('Ctrl Pts',(-1.11293079588184,2.18770396700547,8.00209115521302));
#9912=CARTESIAN_POINT('Ctrl Pts',(-1.83590515273836,1.81991178007634,8.04443026185436));
#9913=CARTESIAN_POINT('Ctrl Pts',(-2.35852839687711,1.05828654826383,8.08676936849571));
#9914=CARTESIAN_POINT('Ctrl Pts',(-2.4416101127223,0.251403383282412,8.12910847513704));
#9915=CARTESIAN_POINT('Ctrl Pts',(-2.45015526165805,0.168413561173331,8.13346315135402));
#9916=CARTESIAN_POINT('Ctrl Pts',(-2.45405067483897,0.0849449733128952,
8.13781782757099));
#9917=CARTESIAN_POINT('Ctrl Pts',(-2.45347385627323,0.00142195494216932,
8.14217250378797));
#9918=CARTESIAN_POINT('Origin',(0.,0.,0.));
#9919=CARTESIAN_POINT('',(-2.44700919659994,0.0011436434892946,9.05782749621206));
#9920=CARTESIAN_POINT('',(-2.44711631602456,0.0012525846534501,8.94217250378797));
#9921=CARTESIAN_POINT('',(-2.4505,-3.00099698131059E-16,0.));
#9922=CARTESIAN_POINT('Ctrl Pts',(-2.44700919659994,0.0011436434892946,
9.05782749621206));
#9923=CARTESIAN_POINT('Ctrl Pts',(-2.44842479019009,0.336683737405834,9.04045091225821));
#9924=CARTESIAN_POINT('Ctrl Pts',(-2.38417117353217,0.67170491204158,9.02307432830436));
#9925=CARTESIAN_POINT('Ctrl Pts',(-2.25164548110497,0.977099482290081,9.00569774435051));
#9926=CARTESIAN_POINT('Ctrl Pts',(-1.92885831958852,1.7209359766906,8.96337434193255));
#9927=CARTESIAN_POINT('Ctrl Pts',(-1.20105210951221,2.28901482807564,8.92105093951459));
#9928=CARTESIAN_POINT('Ctrl Pts',(-0.401097684339819,2.42151841175928,8.87872753709663));
#9929=CARTESIAN_POINT('Ctrl Pts',(0.398856740832569,2.55402199544293,8.83640413467867));
#9930=CARTESIAN_POINT('Ctrl Pts',(1.27095938110103,2.25095031142518,8.7940807322607));
#9931=CARTESIAN_POINT('Ctrl Pts',(1.81634371305176,1.65091680194046,8.75175732984274));
#9932=CARTESIAN_POINT('Ctrl Pts',(2.36172804500248,1.05088329245573,8.70943392742478));
#9933=CARTESIAN_POINT('Ctrl Pts',(2.58039406863547,0.153887957504024,8.66711052500682));
#9934=CARTESIAN_POINT('Ctrl Pts',(2.37233227519797,-0.6298177092826,8.62478712258885));
#9935=CARTESIAN_POINT('Ctrl Pts',(2.16427048176047,-1.41352337606922,8.58246372017089));
#9936=CARTESIAN_POINT('Ctrl Pts',(1.5294808712525,-2.08393937469077,8.54014031775292));
#9937=CARTESIAN_POINT('Ctrl Pts',(0.758292028122076,-2.33444296802438,8.49781691533496));
#9938=CARTESIAN_POINT('Ctrl Pts',(-0.0128968150083492,-2.58494656135799,
8.455493512917));
#9939=CARTESIAN_POINT('Ctrl Pts',(-0.920484890761226,-2.41553774940367,
8.41317011049905));
#9940=CARTESIAN_POINT('Ctrl Pts',(-1.54937598941065,-1.90369766883025,8.37084670808108));
#9941=CARTESIAN_POINT('Ctrl Pts',(-2.10916696603463,-1.44809659704721,8.33317363745808));
#9942=CARTESIAN_POINT('Ctrl Pts',(-2.44814061482272,-0.72118021180151,8.29550056683506));
#9943=CARTESIAN_POINT('Ctrl Pts',(-2.45333810822071,0.00149720406526131,
8.25782749621206));
#9944=CARTESIAN_POINT('Ctrl Pts',(-2.45347385627323,0.00142195494216932,
8.14217250378797));
#9945=CARTESIAN_POINT('Ctrl Pts',(-2.44844245472095,-0.727122286250471,
8.18015693421233));
#9946=CARTESIAN_POINT('Ctrl Pts',(-2.1031409456273,-1.45980787714039,8.21814136463669));
#9947=CARTESIAN_POINT('Ctrl Pts',(-1.53537261678876,-1.91501815429747,8.25612579506105));
#9948=CARTESIAN_POINT('Ctrl Pts',(-0.902513217458377,-2.42241542874561,
8.29846490170239));
#9949=CARTESIAN_POINT('Ctrl Pts',(0.00674576875401803,-2.58506887949157,
8.34080400834373));
#9950=CARTESIAN_POINT('Ctrl Pts',(0.77626128426866,-2.32853645499039,8.38314311498507));
#9951=CARTESIAN_POINT('Ctrl Pts',(1.5457767997833,-2.07200403048922,8.42548222162641));
#9952=CARTESIAN_POINT('Ctrl Pts',(2.17554884460018,-1.39628573074092,8.46782132826775));
#9953=CARTESIAN_POINT('Ctrl Pts',(2.37734791724352,-0.610639405911168,8.51016043490908));
#9954=CARTESIAN_POINT('Ctrl Pts',(2.57914698988687,0.175006918918576,8.55249954155042));
#9955=CARTESIAN_POINT('Ctrl Pts',(2.35297309035668,1.07058126882979,8.59483864819176));
#9956=CARTESIAN_POINT('Ctrl Pts',(1.80233984845749,1.66620367132469,8.6371777548331));
#9957=CARTESIAN_POINT('Ctrl Pts',(1.2517066065583,2.2618260738196,8.67951686147444));
#9958=CARTESIAN_POINT('Ctrl Pts',(0.376614022290118,2.5574965288982,8.72185596811578));
#9959=CARTESIAN_POINT('Ctrl Pts',(-0.422431877786136,2.41789472729971,8.76419507475712));
#9960=CARTESIAN_POINT('Ctrl Pts',(-1.2214777778624,2.27829292570122,8.80653418139846));
#9961=CARTESIAN_POINT('Ctrl Pts',(-1.94447699374672,1.70341886742563,8.8488732880398));
#9962=CARTESIAN_POINT('Ctrl Pts',(-2.26053248852424,0.956376741666199,8.89121239468114));
#9963=CARTESIAN_POINT('Ctrl Pts',(-2.38733584500595,0.656658968854799,8.90819909771675));
#9964=CARTESIAN_POINT('Ctrl Pts',(-2.4486349994353,0.32922794899108,8.92518580075236));
#9965=CARTESIAN_POINT('Ctrl Pts',(-2.44711631602456,0.0012525846534501,
8.94217250378797));
#9966=CARTESIAN_POINT('Origin',(0.,0.,0.));
#9967=CARTESIAN_POINT('',(-2.44916657089282,-0.00214086048378637,9.85782749621207));
#9968=CARTESIAN_POINT('',(-2.44890296710392,-0.00209289085269487,9.74217250378797));
#9969=CARTESIAN_POINT('',(-2.4505,-3.00099698131059E-16,0.));
#9970=CARTESIAN_POINT('Ctrl Pts',(-2.44916657089282,-0.00214086048378637,
9.85782749621207));
#9971=CARTESIAN_POINT('Ctrl Pts',(-2.4443000397846,0.577853720703854,9.82772466009932));
#9972=CARTESIAN_POINT('Ctrl Pts',(-2.23817293760382,1.16095889116584,9.79762182398657));
#9973=CARTESIAN_POINT('Ctrl Pts',(-1.86255786053494,1.59859594239178,9.76751898787382));
#9974=CARTESIAN_POINT('Ctrl Pts',(-1.33445785024021,2.21389640652993,9.72519558545586));
#9975=CARTESIAN_POINT('Ctrl Pts',(-0.471326673231223,2.54164636014034,9.68287218303791));
#9976=CARTESIAN_POINT('Ctrl Pts',(0.332072352589864,2.43194546063792,9.64054878061995));
#9977=CARTESIAN_POINT('Ctrl Pts',(1.13547137841094,2.3222445611355,9.59822537820198));
#9978=CARTESIAN_POINT('Ctrl Pts',(1.87913825304411,1.77509280852021,9.55590197578401));
#9979=CARTESIAN_POINT('Ctrl Pts',(2.22294807929644,1.04073656975442,9.51357857336605));
#9980=CARTESIAN_POINT('Ctrl Pts',(2.56675790554877,0.306380330988639,9.47125517094809));
#9981=CARTESIAN_POINT('Ctrl Pts',(2.51071068342031,-0.615180393927636,9.42893176853014));
#9982=CARTESIAN_POINT('Ctrl Pts',(2.08044027709761,-1.30245883785323,9.38660836611217));
#9983=CARTESIAN_POINT('Ctrl Pts',(1.65016987077491,-1.98973728177882,9.34428496369421));
#9984=CARTESIAN_POINT('Ctrl Pts',(0.845676280257953,-2.44273344471371,9.30196156127624));
#9985=CARTESIAN_POINT('Ctrl Pts',(0.0349042252868802,-2.45426413939679,
9.25963815885828));
#9986=CARTESIAN_POINT('Ctrl Pts',(-0.775867829684193,-2.46579483407987,
9.21731475644032));
#9987=CARTESIAN_POINT('Ctrl Pts',(-1.5929183491094,-2.03586006051114,9.17499135402236));
#9988=CARTESIAN_POINT('Ctrl Pts',(-2.0425595523437,-1.36109560501879,9.1326679516044));
#9989=CARTESIAN_POINT('Ctrl Pts',(-2.30759300500181,-0.963367033696284,
9.10772113314029));
#9990=CARTESIAN_POINT('Ctrl Pts',(-2.44497688942113,-0.480576919804305,
9.08277431467618));
#9991=CARTESIAN_POINT('Ctrl Pts',(-2.44700919659994,0.0011436434892946,
9.05782749621206));
#9992=CARTESIAN_POINT('Ctrl Pts',(-2.44711631602456,0.0012525846534501,
8.94217250378797));
#9993=CARTESIAN_POINT('Ctrl Pts',(-2.44484970344542,-0.488245806646622,
8.9675249073937));
#9994=CARTESIAN_POINT('Ctrl Pts',(-2.30265559068752,-0.978956731903437,
8.99287731099942));
#9995=CARTESIAN_POINT('Ctrl Pts',(-2.02946487371307,-1.38055638423009,9.01822971460515));
#9996=CARTESIAN_POINT('Ctrl Pts',(-1.57322999045366,-2.0512371911237,9.06056882124649));
#9997=CARTESIAN_POINT('Ctrl Pts',(-0.751648450264089,-2.4733886116677,9.10290792788784));
#9998=CARTESIAN_POINT('Ctrl Pts',(0.0592642668109431,-2.45380344574561,
9.14524703452917));
#9999=CARTESIAN_POINT('Ctrl Pts',(0.870176983885975,-2.43421827982352,9.18758614117051));
#10000=CARTESIAN_POINT('Ctrl Pts',(1.67042087784649,-1.97289652743534,9.22992524781184));
#10001=CARTESIAN_POINT('Ctrl Pts',(2.09374612780316,-1.28097258205744,9.27226435445318));
#10002=CARTESIAN_POINT('Ctrl Pts',(2.51707137775985,-0.589048636679533,
9.31460346109452));
#10003=CARTESIAN_POINT('Ctrl Pts',(2.56347798371271,0.333477501688088,9.35694256773587));
#10004=CARTESIAN_POINT('Ctrl Pts',(2.21172690685546,1.06439076149939,9.39928167437721));
#10005=CARTESIAN_POINT('Ctrl Pts',(1.85997582999822,1.79530402131068,9.44162078101855));
#10006=CARTESIAN_POINT('Ctrl Pts',(1.11006707033088,2.33460440256564,9.48395988765988));
#10007=CARTESIAN_POINT('Ctrl Pts',(0.305213429580908,2.43546881853928,9.52629899430122));
#10008=CARTESIAN_POINT('Ctrl Pts',(-0.499640211169086,2.53633323451293,
9.56863810094255));
#10009=CARTESIAN_POINT('Ctrl Pts',(-1.35943873300173,2.19876168520523,9.6109772075839));
#10010=CARTESIAN_POINT('Ctrl Pts',(-1.88067578491744,1.57725146875786,9.65331631422524));
#10011=CARTESIAN_POINT('Ctrl Pts',(-2.24531218505443,1.14246801055816,9.68293504407948));
#10012=CARTESIAN_POINT('Ctrl Pts',(-2.44426212764736,0.568729602967145,
9.71255377393372));
#10013=CARTESIAN_POINT('Ctrl Pts',(-2.44890296710392,-0.00209289085269486,
9.74217250378797));
#10014=CARTESIAN_POINT('Origin',(0.,0.,0.));
#10015=CARTESIAN_POINT('',(-2.45449565980291,0.000180539251598464,10.6578274962121));
#10016=CARTESIAN_POINT('',(-2.45451849884274,-3.1633834378794E-5,10.542172503788));
#10017=CARTESIAN_POINT('',(-2.4505,-3.00099698131059E-16,0.));
#10018=CARTESIAN_POINT('Ctrl Pts',(-2.45449565980291,0.000180539251598464,
10.6578274962121));
#10019=CARTESIAN_POINT('Ctrl Pts',(-2.45450594062414,0.00986891292668717,
10.6573218103584));
#10020=CARTESIAN_POINT('Ctrl Pts',(-2.45445353368688,0.0195571722527011,
10.6568161245047));
#10021=CARTESIAN_POINT('Ctrl Pts',(-2.45433810212205,0.0292446806083813,
10.656310438651));
#10022=CARTESIAN_POINT('Ctrl Pts',(-2.44467705162092,0.840041169343448,
10.6139870362331));
#10023=CARTESIAN_POINT('Ctrl Pts',(-1.99353722868095,1.6455772150759,10.5716636338151));
#10024=CARTESIAN_POINT('Ctrl Pts',(-1.30725280137001,2.07743131876416,10.5293402313971));
#10025=CARTESIAN_POINT('Ctrl Pts',(-0.620968374059076,2.50928542245243,
10.4870168289792));
#10026=CARTESIAN_POINT('Ctrl Pts',(0.300460657622818,2.56745758409652,10.4446934265612));
#10027=CARTESIAN_POINT('Ctrl Pts',(1.03560775800279,2.22534207312862,10.4023700241433));
#10028=CARTESIAN_POINT('Ctrl Pts',(1.77075485838276,1.88322656216073,10.3600466217253));
#10029=CARTESIAN_POINT('Ctrl Pts',(2.31962002746079,1.14082337858087,10.3177232193073));
#10030=CARTESIAN_POINT('Ctrl Pts',(2.43117324686004,0.337679455436603,10.2753998168894));
#10031=CARTESIAN_POINT('Ctrl Pts',(2.54272646625929,-0.46546446770764,10.2330764144714));
#10032=CARTESIAN_POINT('Ctrl Pts',(2.21696773597977,-1.3293491304163,10.1907530120535));
#10033=CARTESIAN_POINT('Ctrl Pts',(1.60288668891411,-1.85886659913344,10.1484296096355));
#10034=CARTESIAN_POINT('Ctrl Pts',(0.988805641848436,-2.3883840678506,10.1061062072175));
#10035=CARTESIAN_POINT('Ctrl Pts',(0.086402277996615,-2.58353434257624,
10.0637828047996));
#10036=CARTESIAN_POINT('Ctrl Pts',(-0.691598482618519,-2.3550631222351,
10.0214594023816));
#10037=CARTESIAN_POINT('Ctrl Pts',(-1.46959924323365,-2.12659190189395,
9.97913599996364));
#10038=CARTESIAN_POINT('Ctrl Pts',(-2.12319740061209,-1.47449918648602,
9.93681259754568));
#10039=CARTESIAN_POINT('Ctrl Pts',(-2.35346205751109,-0.697027341449118,
9.89448919512772));
#10040=CARTESIAN_POINT('Ctrl Pts',(-2.41994925718359,-0.472538153673385,
9.8822686288225));
#10041=CARTESIAN_POINT('Ctrl Pts',(-2.45114219092616,-0.237595825907136,
9.87004806251728));
#10042=CARTESIAN_POINT('Ctrl Pts',(-2.44916657089282,-0.00214086048378637,
9.85782749621207));
#10043=CARTESIAN_POINT('Ctrl Pts',(-2.44890296710392,-0.00209289085269486,
9.74217250378797));
#10044=CARTESIAN_POINT('Ctrl Pts',(-2.45089607169639,-0.247244429614459,
9.75489288057506));
#10045=CARTESIAN_POINT('Ctrl Pts',(-2.41704981698823,-0.491858142409003,
9.76761325736216));
#10046=CARTESIAN_POINT('Ctrl Pts',(-2.3450968955658,-0.724695904556749,
9.78033363414925));
#10047=CARTESIAN_POINT('Ctrl Pts',(-2.10560537229968,-1.49968417783698,
9.82267274079059));
#10048=CARTESIAN_POINT('Ctrl Pts',(-1.44394674376867,-2.14421184081045,
9.86501184743193));
#10049=CARTESIAN_POINT('Ctrl Pts',(-0.6629441317963,-2.36329614771203,9.90735095407327));
#10050=CARTESIAN_POINT('Ctrl Pts',(0.118058480176069,-2.58238045461361,
9.94969006071461));
#10051=CARTESIAN_POINT('Ctrl Pts',(1.01840507558981,-2.37602140544331,9.99202916735595));
#10052=CARTESIAN_POINT('Ctrl Pts',(1.62603155524061,-1.83866391301822,10.0343682739973));
#10053=CARTESIAN_POINT('Ctrl Pts',(2.23365803489143,-1.30130642059312,10.0767073806386));
#10054=CARTESIAN_POINT('Ctrl Pts',(2.5485643987793,-0.432950484913232,10.11904648728));
#10055=CARTESIAN_POINT('Ctrl Pts',(2.42662658642559,0.368981047922729,10.1613855939213));
#10056=CARTESIAN_POINT('Ctrl Pts',(2.30468877407188,1.17091258075867,10.2037247005626));
#10057=CARTESIAN_POINT('Ctrl Pts',(1.74590678547659,1.90641971075067,10.246063807204));
#10058=CARTESIAN_POINT('Ctrl Pts',(1.00601990810412,2.23888086958012,10.2884029138453));
#10059=CARTESIAN_POINT('Ctrl Pts',(0.266133030731654,2.57134202840957,10.3307420204867));
#10060=CARTESIAN_POINT('Ctrl Pts',(-0.654858735418012,2.50075721607648,
10.373081127128));
#10061=CARTESIAN_POINT('Ctrl Pts',(-1.33544255914608,2.05943117750874,10.4154202337693));
#10062=CARTESIAN_POINT('Ctrl Pts',(-2.01460619326385,1.61902606393638,10.4576709904422));
#10063=CARTESIAN_POINT('Ctrl Pts',(-2.45436416747304,0.809425377921695,
10.4999217471151));
#10064=CARTESIAN_POINT('Ctrl Pts',(-2.45451849884274,-3.1633834378794E-5,
10.542172503788));
#10065=CARTESIAN_POINT('Origin',(0.,0.,0.));
#10066=CARTESIAN_POINT('',(-2.44864274206392,0.00202326491164903,11.4578274962121));
#10067=CARTESIAN_POINT('',(-2.44899529462048,0.00211273287450485,11.342172503788));
#10068=CARTESIAN_POINT('',(-2.4505,-3.00099698131059E-16,0.));
#10069=CARTESIAN_POINT('Ctrl Pts',(-2.44864274206392,0.00202326491164903,
11.4578274962121));
#10070=CARTESIAN_POINT('Ctrl Pts',(-2.45063313417738,0.25710244065764,11.4445955581995));
#10071=CARTESIAN_POINT('Ctrl Pts',(-2.41394631700749,0.511623348699365,
11.4313636201869));
#10072=CARTESIAN_POINT('Ctrl Pts',(-2.33618535765509,0.752906863795201,
11.4181316821743));
#10073=CARTESIAN_POINT('Ctrl Pts',(-2.08746076629505,1.52467130952633,11.3758082797564));
#10074=CARTESIAN_POINT('Ctrl Pts',(-1.41851035397114,2.16100518939464,11.3334848773384));
#10075=CARTESIAN_POINT('Ctrl Pts',(-0.63528655446768,2.37087362897826,11.2911614749205));
#10076=CARTESIAN_POINT('Ctrl Pts',(0.147937245035775,2.58074206856189,11.2488380725025));
#10077=CARTESIAN_POINT('Ctrl Pts',(1.04543443171877,2.36414506786083,11.2065146700845));
#10078=CARTESIAN_POINT('Ctrl Pts',(1.64672398408625,1.82014584336175,11.1641912676666));
#10079=CARTESIAN_POINT('Ctrl Pts',(2.24801353645374,1.27614661886266,11.1218678652486));
#10080=CARTESIAN_POINT('Ctrl Pts',(2.55309545450571,0.404745170565546,11.0795444628307));
#10081=CARTESIAN_POINT('Ctrl Pts',(2.42243689154382,-0.395512676610367,
11.0372210604127));
#10082=CARTESIAN_POINT('Ctrl Pts',(2.29177832858192,-1.19577052378629,10.9948976579947));
#10083=CARTESIAN_POINT('Ctrl Pts',(1.72537928460614,-1.92488476984101,10.9525742555768));
#10084=CARTESIAN_POINT('Ctrl Pts',(0.982289104388552,-2.24938633548608,
10.9102508531588));
#10085=CARTESIAN_POINT('Ctrl Pts',(0.239198924170983,-2.57388790113114,
10.8679274507408));
#10086=CARTESIAN_POINT('Ctrl Pts',(-0.680582392288389,-2.49377678636659,
10.8256040483229));
#10087=CARTESIAN_POINT('Ctrl Pts',(-1.35638191148693,-2.04569276311548,
10.7832806459049));
#10088=CARTESIAN_POINT('Ctrl Pts',(-2.02410688475446,-1.60296250961991,
10.7414629293406));
#10089=CARTESIAN_POINT('Ctrl Pts',(-2.45364548678456,-0.800999998758872,
10.6996452127763));
#10090=CARTESIAN_POINT('Ctrl Pts',(-2.45449565980291,0.000180539251598464,
10.6578274962121));
#10091=CARTESIAN_POINT('Ctrl Pts',(-2.45451849884274,-3.1633834378794E-5,
10.542172503788));
#10092=CARTESIAN_POINT('Ctrl Pts',(-2.45467347565279,-0.812873934143394,
10.5845999603978));
#10093=CARTESIAN_POINT('Ctrl Pts',(-2.01069613156042,-1.6255695989997,10.6270274170076));
#10094=CARTESIAN_POINT('Ctrl Pts',(-1.32685678597742,-2.06497328631131,
10.6694548736174));
#10095=CARTESIAN_POINT('Ctrl Pts',(-0.64444145185873,-2.50346196940119,
10.7117939802587));
#10096=CARTESIAN_POINT('Ctrl Pts',(0.276836203683142,-2.57021172930212,
10.7541330869));
#10097=CARTESIAN_POINT('Ctrl Pts',(1.01533250566608,-2.23467302006614,10.7964721935414));
#10098=CARTESIAN_POINT('Ctrl Pts',(1.753828807649,-1.89913431083016,10.8388113001827));
#10099=CARTESIAN_POINT('Ctrl Pts',(2.30954375607297,-1.1613071324573,10.8811504068241));
#10100=CARTESIAN_POINT('Ctrl Pts',(2.42814176417273,-0.358874876180815,
10.9234895134654));
#10101=CARTESIAN_POINT('Ctrl Pts',(2.54673977227249,0.44355738009568,10.9658286201067));
#10102=CARTESIAN_POINT('Ctrl Pts',(2.22822084004799,1.31059471427581,11.0081677267481));
#10103=CARTESIAN_POINT('Ctrl Pts',(1.61836240205076,1.84541776823085,11.0505068333894));
#10104=CARTESIAN_POINT('Ctrl Pts',(1.00850396405353,2.3802408221859,11.0928459400307));
#10105=CARTESIAN_POINT('Ctrl Pts',(0.107306020283557,2.58284959591588,11.1351850466721));
#10106=CARTESIAN_POINT('Ctrl Pts',(-0.67277769111436,2.36051557546492,11.1775241533134));
#10107=CARTESIAN_POINT('Ctrl Pts',(-1.45286140251225,2.13818155501397,11.2198632599548));
#10108=CARTESIAN_POINT('Ctrl Pts',(-2.11183088153809,1.49090474038213,11.2622023665961));
#10109=CARTESIAN_POINT('Ctrl Pts',(-2.34809375680837,0.714926089124754,
11.3045414732374));
#10110=CARTESIAN_POINT('Ctrl Pts',(-2.41809063190044,0.485029281748485,
11.3170851500876));
#10111=CARTESIAN_POINT('Ctrl Pts',(-2.45098481963534,0.243835787818979,
11.3296288269378));
#10112=CARTESIAN_POINT('Ctrl Pts',(-2.44899529462048,0.00211273287450485,
11.342172503788));
#10113=CARTESIAN_POINT('Origin',(0.,0.,0.));
#10114=CARTESIAN_POINT('',(-2.44731685610913,-0.00140773067336952,12.2578274962121));
#10115=CARTESIAN_POINT('',(-2.4470647235883,-0.0012054690616184,12.142172503788));
#10116=CARTESIAN_POINT('',(-2.4505,-3.00099698131059E-16,0.));
#10117=CARTESIAN_POINT('Ctrl Pts',(-2.44731685610913,-0.00140773067336952,
12.2578274962121));
#10118=CARTESIAN_POINT('Ctrl Pts',(-2.4446942722333,0.499684558237575,12.2318693060406));
#10119=CARTESIAN_POINT('Ctrl Pts',(-2.29510898968982,1.00221422879886,12.2059111158691));
#10120=CARTESIAN_POINT('Ctrl Pts',(-2.00954795106829,1.40937851666229,12.1799529256977));
#10121=CARTESIAN_POINT('Ctrl Pts',(-1.54395637196988,2.0732375103609,12.1376295232797));
#10122=CARTESIAN_POINT('Ctrl Pts',(-0.716893501761423,2.48358184081904,
12.0953061208618));
#10123=CARTESIAN_POINT('Ctrl Pts',(0.0933736111014519,2.4527356440558,12.0529827184438));
#10124=CARTESIAN_POINT('Ctrl Pts',(0.903640723964315,2.42188944729257,12.0106593160258));
#10125=CARTESIAN_POINT('Ctrl Pts',(1.6971120794816,1.94985272330796,11.9683359136078));
#10126=CARTESIAN_POINT('Ctrl Pts',(2.11088410829111,1.25251708660442,11.9260125111899));
#10127=CARTESIAN_POINT('Ctrl Pts',(2.52465613710063,0.55518144990085,11.8836891087719));
#10128=CARTESIAN_POINT('Ctrl Pts',(2.55872883920235,-0.367453099521673,
11.841365706354));
#10129=CARTESIAN_POINT('Ctrl Pts',(2.19751865871293,-1.09340866810195,11.799042303936));
#10130=CARTESIAN_POINT('Ctrl Pts',(1.83630847822352,-1.81936423668222,11.7567189015181));
#10131=CARTESIAN_POINT('Ctrl Pts',(1.07981541514298,-2.34864082442025,11.7143954991001));
#10132=CARTESIAN_POINT('Ctrl Pts',(0.274030576624401,-2.43916748378353,
11.6720720966821));
#10133=CARTESIAN_POINT('Ctrl Pts',(-0.531754261894183,-2.5296941431468,
11.6297486942642));
#10134=CARTESIAN_POINT('Ctrl Pts',(-1.38683087585082,-2.18147087413532,
11.5874252918462));
#10135=CARTESIAN_POINT('Ctrl Pts',(-1.90011979763105,-1.5537617338326,11.5451018894282));
#10136=CARTESIAN_POINT('Ctrl Pts',(-2.25293468359385,-1.12229882988837,
11.5160104250228));
#10137=CARTESIAN_POINT('Ctrl Pts',(-2.44426670725582,-0.558788519025065,
11.4869189606174));
#10138=CARTESIAN_POINT('Ctrl Pts',(-2.44864274206392,0.00202326491164903,
11.4578274962121));
#10139=CARTESIAN_POINT('Ctrl Pts',(-2.44899529462048,0.00211273287450485,
11.342172503788));
#10140=CARTESIAN_POINT('Ctrl Pts',(-2.44426950699009,-0.572060406192228,
11.3719679335791));
#10141=CARTESIAN_POINT('Ctrl Pts',(-2.24272232871244,-1.14922144210772,
11.4017633633703));
#10142=CARTESIAN_POINT('Ctrl Pts',(-1.87409278465252,-1.58506777084989,
11.4315587931615));
#10143=CARTESIAN_POINT('Ctrl Pts',(-1.35027266571165,-2.20440249168428,
11.4738978998028));
#10144=CARTESIAN_POINT('Ctrl Pts',(-0.489076156315162,-2.53839144547012,
11.5162370064441));
#10145=CARTESIAN_POINT('Ctrl Pts',(0.315350571729276,-2.43417699039813,
11.5585761130855));
#10146=CARTESIAN_POINT('Ctrl Pts',(1.1197772997737,-2.32996253532614,11.6009152197268));
#10147=CARTESIAN_POINT('Ctrl Pts',(1.8674342464661,-1.78754467139634,11.6432543263682));
#10148=CARTESIAN_POINT('Ctrl Pts',(2.21613920350807,-1.05517327219197,11.6855934330095));
#10149=CARTESIAN_POINT('Ctrl Pts',(2.56484416055002,-0.322801872987598,
11.7279325396508));
#10150=CARTESIAN_POINT('Ctrl Pts',(2.51459712794155,0.599523061491336,11.7702716462922));
#10151=CARTESIAN_POINT('Ctrl Pts',(2.08839480310448,1.28967854523516,11.8126107529335));
#10152=CARTESIAN_POINT('Ctrl Pts',(1.66219247826739,1.97983402897899,11.8549498595748));
#10153=CARTESIAN_POINT('Ctrl Pts',(0.860034861201667,2.4378200619877,11.8972889662162));
#10154=CARTESIAN_POINT('Ctrl Pts',(0.0490476317064056,2.45402891863516,
11.9396280728575));
#10155=CARTESIAN_POINT('Ctrl Pts',(-0.761939597788844,2.47023777528262,
11.9819671794989));
#10156=CARTESIAN_POINT('Ctrl Pts',(-1.58175643971363,2.04466945556887,12.0243062861402));
#10157=CARTESIAN_POINT('Ctrl Pts',(-2.03519506832506,1.37209498123819,12.0666453927815));
#10158=CARTESIAN_POINT('Ctrl Pts',(-2.30481900353504,0.972168364826713,
12.0918210964503));
#10159=CARTESIAN_POINT('Ctrl Pts',(-2.44490126731575,0.484906887990491,
12.1169968001192));
#10160=CARTESIAN_POINT('Ctrl Pts',(-2.4470647235883,-0.0012054690616184,
12.142172503788));
#10161=CARTESIAN_POINT('Origin',(0.,0.,0.));
#10162=CARTESIAN_POINT('',(-2.45375856134309,-0.00121882424236025,13.0578274962121));
#10163=CARTESIAN_POINT('',(-2.45339670897876,-0.00146880086599289,12.942172503788));
#10164=CARTESIAN_POINT('',(-2.4505,-3.00099698131059E-16,0.));
#10165=CARTESIAN_POINT('Ctrl Pts',(-2.45375856134309,-0.00121882424236025,
13.0578274962121));
#10166=CARTESIAN_POINT('Ctrl Pts',(-2.44923208495134,0.740524702851974,
13.0191430538817));
#10167=CARTESIAN_POINT('Ctrl Pts',(-2.08937875229641,1.48607239035232,12.9804586115513));
#10168=CARTESIAN_POINT('Ctrl Pts',(-1.50357549119931,1.94007513079693,12.941774169221));
#10169=CARTESIAN_POINT('Ctrl Pts',(-0.862667010590097,2.4367849067477,12.899450766803));
#10170=CARTESIAN_POINT('Ctrl Pts',(0.0486999946819842,2.58451994835246,
12.8571273643851));
#10171=CARTESIAN_POINT('Ctrl Pts',(0.813700976493747,2.31571187580085,12.8148039619671));
#10172=CARTESIAN_POINT('Ctrl Pts',(1.57870195830553,2.04690380324923,12.7724805595491));
#10173=CARTESIAN_POINT('Ctrl Pts',(2.197336916657,1.3615526165412,12.7301571571312));
#10174=CARTESIAN_POINT('Ctrl Pts',(2.38666578955733,0.573111838848801,12.6878337547132));
#10175=CARTESIAN_POINT('Ctrl Pts',(2.57599466245766,-0.2153289388436,12.6455103522952));
#10176=CARTESIAN_POINT('Ctrl Pts',(2.33601744990688,-1.10685930752036,12.6031869498773));
#10177=CARTESIAN_POINT('Ctrl Pts',(1.77649058658243,-1.69372724092635,12.5608635474593));
#10178=CARTESIAN_POINT('Ctrl Pts',(1.216963723258,-2.28059517433232,12.5185401450414));
#10179=CARTESIAN_POINT('Ctrl Pts',(0.337887209159924,-2.56280067246752,
12.4762167426234));
#10180=CARTESIAN_POINT('Ctrl Pts',(-0.458682848089992,-2.41127369158709,
12.4338933402054));
#10181=CARTESIAN_POINT('Ctrl Pts',(-1.25525290533992,-2.25974671070665,
12.3915699377875));
#10182=CARTESIAN_POINT('Ctrl Pts',(-1.9693165057417,-1.67448725081058,12.3492465353695));
#10183=CARTESIAN_POINT('Ctrl Pts',(-2.27428816194839,-0.923170692393001,
12.3069231329516));
#10184=CARTESIAN_POINT('Ctrl Pts',(-2.39221171246308,-0.632658724064287,
12.2905579207051));
#10185=CARTESIAN_POINT('Ctrl Pts',(-2.44897025110618,-0.317318878906041,
12.2741927084586));
#10186=CARTESIAN_POINT('Ctrl Pts',(-2.44731685610913,-0.00140773067336952,
12.2578274962121));
#10187=CARTESIAN_POINT('Ctrl Pts',(-2.4470647235883,-0.0012054690616184,
12.142172503788));
#10188=CARTESIAN_POINT('Ctrl Pts',(-2.44853964847253,-0.332610000341817,
12.1593359067605));
#10189=CARTESIAN_POINT('Ctrl Pts',(-2.38591324110648,-0.663480448487108,
12.176499309733));
#10190=CARTESIAN_POINT('Ctrl Pts',(-2.25653113483059,-0.965779913444993,
12.1936627127056));
#10191=CARTESIAN_POINT('Ctrl Pts',(-1.93736815742667,-1.71149970484984,
12.2360018193469));
#10192=CARTESIAN_POINT('Ctrl Pts',(-1.21198178732078,-2.2833586587119,12.2783409259882));
#10193=CARTESIAN_POINT('Ctrl Pts',(-0.412361596856918,-2.41963251695609,
12.3206800326296));
#10194=CARTESIAN_POINT('Ctrl Pts',(0.387258593606936,-2.55590637520028,
12.3630191392709));
#10195=CARTESIAN_POINT('Ctrl Pts',(1.26111260442874,-2.25659513782664,12.4053582459123));
#10196=CARTESIAN_POINT('Ctrl Pts',(1.80926127035868,-1.65868540092863,12.4476973525536));
#10197=CARTESIAN_POINT('Ctrl Pts',(2.3574099362886,-1.06077566403063,12.4900364591949));
#10198=CARTESIAN_POINT('Ctrl Pts',(2.57985325732663,-0.164267427608244,
12.5323755658363));
#10199=CARTESIAN_POINT('Ctrl Pts',(2.37478498777309,0.620531921436152,12.5747146724776));
#10200=CARTESIAN_POINT('Ctrl Pts',(2.16971671821954,1.40533127048057,12.6170537791189));
#10201=CARTESIAN_POINT('Ctrl Pts',(1.53713685807443,2.078421732147,12.6593928857603));
#10202=CARTESIAN_POINT('Ctrl Pts',(0.766559969366697,2.33174814614233,12.7017319924016));
#10203=CARTESIAN_POINT('Ctrl Pts',(-0.00401691934101722,2.58507456013765,
12.744071099043));
#10204=CARTESIAN_POINT('Ctrl Pts',(-0.912590836611347,2.41863692646186,
12.7864102056843));
#10205=CARTESIAN_POINT('Ctrl Pts',(-1.54333226224883,1.90860921405498,12.8287493123256));
#10206=CARTESIAN_POINT('Ctrl Pts',(-2.10656809123738,1.45316761829443,12.8665570428131));
#10207=CARTESIAN_POINT('Ctrl Pts',(-2.44825947251039,0.723746281051334,
12.9043647733005));
#10208=CARTESIAN_POINT('Ctrl Pts',(-2.45339670897876,-0.00146880086599289,
12.942172503788));
#10209=CARTESIAN_POINT('Origin',(0.,0.,0.));
#10210=CARTESIAN_POINT('',(-2.45094795586712,0.0022061736527193,13.8578274962121));
#10211=CARTESIAN_POINT('',(-2.45152510826581,0.00213207818356079,13.742172503788));
#10212=CARTESIAN_POINT('',(-2.4505,-3.00099698131059E-16,0.));
#10213=CARTESIAN_POINT('Ctrl Pts',(-2.45094795586712,0.0022061736527193,
13.8578274962121));
#10214=CARTESIAN_POINT('Ctrl Pts',(-2.45256019575125,0.176967728202779,
13.8487402041408));
#10215=CARTESIAN_POINT('Ctrl Pts',(-2.43545641918873,0.351416146632857,
13.8396529120695));
#10216=CARTESIAN_POINT('Ctrl Pts',(-2.39846348572391,0.52153971902537,13.8305656199982));
#10217=CARTESIAN_POINT('Ctrl Pts',(-2.22617158651246,1.31387789399109,13.7882422175802));
#10218=CARTESIAN_POINT('Ctrl Pts',(-1.62245146862923,2.01240311191786,13.7459188151623));
#10219=CARTESIAN_POINT('Ctrl Pts',(-0.863421714241279,2.29763654964152,
13.7035954127443));
#10220=CARTESIAN_POINT('Ctrl Pts',(-0.104391959853312,2.58286998736519,
13.6612720103263));
#10221=CARTESIAN_POINT('Ctrl Pts',(0.809947431039378,2.45481164488573,13.6189486079084));
#10222=CARTESIAN_POINT('Ctrl Pts',(1.46141245436887,1.97203052945118,13.5766252054904));
#10223=CARTESIAN_POINT('Ctrl Pts',(2.11287747769833,1.48924941401666,13.5343018030724));
#10224=CARTESIAN_POINT('Ctrl Pts',(2.50146813346461,0.651745525627052,13.4919784006545));
#10225=CARTESIAN_POINT('Ctrl Pts',(2.44945785974733,-0.157438763314421,
13.4496549982365));
#10226=CARTESIAN_POINT('Ctrl Pts',(2.39744758603005,-0.966623052255928,
13.4073315958186));
#10227=CARTESIAN_POINT('Ctrl Pts',(1.90483638282921,-1.74748774174929,13.3650081934006));
#10228=CARTESIAN_POINT('Ctrl Pts',(1.19692584762066,-2.14289507119913,13.3226847909826));
#10229=CARTESIAN_POINT('Ctrl Pts',(0.489015312412128,-2.53830240064897,
13.2803613885647));
#10230=CARTESIAN_POINT('Ctrl Pts',(-0.434194554804115,-2.54825237005527,
13.2380379861467));
#10231=CARTESIAN_POINT('Ctrl Pts',(-1.1504627320257,-2.16819424247273,13.1957145837288));
#10232=CARTESIAN_POINT('Ctrl Pts',(-1.86673090924731,-1.78813611489019,
13.1533911813108));
#10233=CARTESIAN_POINT('Ctrl Pts',(-2.37605739647428,-1.0180698903188,13.1110677788928));
#10234=CARTESIAN_POINT('Ctrl Pts',(-2.44549566211458,-0.210194522884695,
13.0687443764749));
#10235=CARTESIAN_POINT('Ctrl Pts',(-2.45146595426458,-0.140733514319843,
13.0651054163873));
#10236=CARTESIAN_POINT('Ctrl Pts',(-2.4541843569843,-0.0709930003124499,
13.0614664562997));
#10237=CARTESIAN_POINT('Ctrl Pts',(-2.45375856134309,-0.00121882424236025,
13.0578274962121));
#10238=CARTESIAN_POINT('Ctrl Pts',(-2.45339670897876,-0.00146880086599289,
12.942172503788));
#10239=CARTESIAN_POINT('Ctrl Pts',(-2.45401242302797,-0.0883881236149842,
12.9467038799419));
#10240=CARTESIAN_POINT('Ctrl Pts',(-2.44979361045224,-0.17524702442689,
12.9512352560958));
#10241=CARTESIAN_POINT('Ctrl Pts',(-2.44054226314134,-0.261566560352387,
12.9557666322497));
#10242=CARTESIAN_POINT('Ctrl Pts',(-2.35410190439172,-1.06809683121483,
12.998105738891));
#10243=CARTESIAN_POINT('Ctrl Pts',(-1.82831225288784,-1.82753958180174,
13.0404448455323));
#10244=CARTESIAN_POINT('Ctrl Pts',(-1.10381290256112,-2.19231856257553,
13.0827839521737));
#10245=CARTESIAN_POINT('Ctrl Pts',(-0.379313552234399,-2.55709754334934,
13.125123058815));
#10246=CARTESIAN_POINT('Ctrl Pts',(0.543895496915153,-2.52721275431003,
13.1674621654564));
#10247=CARTESIAN_POINT('Ctrl Pts',(1.24328662368826,-2.11634164893845,13.2098012720977));
#10248=CARTESIAN_POINT('Ctrl Pts',(1.94267775046136,-1.70547054356687,13.252140378739));
#10249=CARTESIAN_POINT('Ctrl Pts',(2.41825095485799,-0.913613121863004,
13.2944794853804));
#10250=CARTESIAN_POINT('Ctrl Pts',(2.45234934221823,-0.103180944924282,
13.3368185920217));
#10251=CARTESIAN_POINT('Ctrl Pts',(2.48644772957847,0.707251232014451,13.379157698663));
#10252=CARTESIAN_POINT('Ctrl Pts',(2.07907129990229,1.53625816418806,13.4214968053044));
#10253=CARTESIAN_POINT('Ctrl Pts',(1.41666514265488,2.00442597200802,13.4638359119457));
#10254=CARTESIAN_POINT('Ctrl Pts',(0.75425898540748,2.47259377982796,13.5061750185871));
#10255=CARTESIAN_POINT('Ctrl Pts',(-0.163176899411125,2.57992246329428,
13.5485141252284));
#10256=CARTESIAN_POINT('Ctrl Pts',(-0.915757110577525,2.27729060905725,
13.5908532318697));
#10257=CARTESIAN_POINT('Ctrl Pts',(-1.66833732174391,1.97465875482023,13.6331923385111));
#10258=CARTESIAN_POINT('Ctrl Pts',(-2.25606185925809,1.26206636287986,13.6755314451524));
#10259=CARTESIAN_POINT('Ctrl Pts',(-2.40994521979868,0.465647550453306,
13.7178705517938));
#10260=CARTESIAN_POINT('Ctrl Pts',(-2.43938739384867,0.313270443469298,
13.7259712024585));
#10261=CARTESIAN_POINT('Ctrl Pts',(-2.45294822593746,0.157824757199172,
13.7340718531232));
#10262=CARTESIAN_POINT('Ctrl Pts',(-2.45152510826581,0.00213207818356079,
13.742172503788));
#10263=CARTESIAN_POINT('Origin',(0.,0.,0.));
#10264=CARTESIAN_POINT('',(-2.44650205703081,-0.000206129442867353,14.6578274962121));
#10265=CARTESIAN_POINT('',(-2.44648675330186,0.00013847494270713,14.542172503788));
#10266=CARTESIAN_POINT('',(-2.4505,-3.00099698131059E-16,0.));
#10267=CARTESIAN_POINT('Ctrl Pts',(-2.44650205703081,-0.000206129442867353,
14.6578274962121));
#10268=CARTESIAN_POINT('Ctrl Pts',(-2.44618553699062,0.42122938413429,14.6360139519819));
#10269=CARTESIAN_POINT('Ctrl Pts',(-2.34285183903272,0.842810353195403,
14.6142004077517));
#10270=CARTESIAN_POINT('Ctrl Pts',(-2.13738885427315,1.20673097934083,14.5923868635215));
#10271=CARTESIAN_POINT('Ctrl Pts',(-1.73874237600212,1.91282252255884,14.5500634611035));
#10272=CARTESIAN_POINT('Ctrl Pts',(-0.955628979015579,2.40185101689915,
14.5077400586856));
#10273=CARTESIAN_POINT('Ctrl Pts',(-0.146214897047949,2.45015345942927,
14.4654166562676));
#10274=CARTESIAN_POINT('Ctrl Pts',(0.663199184919693,2.49845590195939,14.4230932538497));
#10275=CARTESIAN_POINT('Ctrl Pts',(1.49891395186842,2.1060322926793,14.3807698514317));
#10276=CARTESIAN_POINT('Ctrl Pts',(1.97870530738246,1.45236224042366,14.3384464490137));
#10277=CARTESIAN_POINT('Ctrl Pts',(2.4584966628965,0.798692188168016,14.2961230465958));
#10278=CARTESIAN_POINT('Ctrl Pts',(2.58236460697585,-0.116224307063184,
14.2537996441778));
#10279=CARTESIAN_POINT('Ctrl Pts',(2.29365666096027,-0.873939295663354,
14.2114762417598));
#10280=CARTESIAN_POINT('Ctrl Pts',(2.00494871494468,-1.63165428426354,14.1691528393419));
#10281=CARTESIAN_POINT('Ctrl Pts',(1.30366487883415,-2.23216776623269,14.1268294369239));
#10282=CARTESIAN_POINT('Ctrl Pts',(0.510545662655815,-2.40082775250856,
14.0845060345059));
#10283=CARTESIAN_POINT('Ctrl Pts',(-0.282573553522497,-2.56948773878442,
14.042182632088));
#10284=CARTESIAN_POINT('Ctrl Pts',(-1.16752814976861,-2.30629422936704,
13.99985922967));
#10285=CARTESIAN_POINT('Ctrl Pts',(-1.73957360762182,-1.73162190865603,
13.9575358272521));
#10286=CARTESIAN_POINT('Ctrl Pts',(-2.18879472110326,-1.28033794817224,
13.9242997169054));
#10287=CARTESIAN_POINT('Ctrl Pts',(-2.44505130565783,-0.636971511603942,
13.8910636065587));
#10288=CARTESIAN_POINT('Ctrl Pts',(-2.45094795586712,0.0022061736527193,
13.8578274962121));
#10289=CARTESIAN_POINT('Ctrl Pts',(-2.45152510826581,0.00213207818356079,
13.742172503788));
#10290=CARTESIAN_POINT('Ctrl Pts',(-2.44551011591929,-0.655923324644509,
13.7764109597646));
#10291=CARTESIAN_POINT('Ctrl Pts',(-2.1718157894574,-1.3183911056973,13.8106494157412));
#10292=CARTESIAN_POINT('Ctrl Pts',(-1.69820083327538,-1.77222389486669,
13.8448878717178));
#10293=CARTESIAN_POINT('Ctrl Pts',(-1.11253090264449,-2.33343129484734,
13.8872269783591));
#10294=CARTESIAN_POINT('Ctrl Pts',(-0.221148857815718,-2.57560086189586,
13.9295660850005));
#10295=CARTESIAN_POINT('Ctrl Pts',(0.567984032494793,-2.38789818512109,
13.9719051916418));
#10296=CARTESIAN_POINT('Ctrl Pts',(1.35711692280528,-2.20019550834633,14.0142442982831));
#10297=CARTESIAN_POINT('Ctrl Pts',(2.04400065859751,-1.58262058774832,14.0565834049245));
#10298=CARTESIAN_POINT('Ctrl Pts',(2.31426727392473,-0.817820633461076,
14.0989225115658));
#10299=CARTESIAN_POINT('Ctrl Pts',(2.58453388925195,-0.0530206791738243,
14.1412616182071));
#10300=CARTESIAN_POINT('Ctrl Pts',(2.43818338411416,0.859004308802644,14.1836007248485));
#10301=CARTESIAN_POINT('Ctrl Pts',(1.94219639616232,1.50084534926412,14.2259398314898));
#10302=CARTESIAN_POINT('Ctrl Pts',(1.44620940821049,2.1426863897256,14.2682789381312));
#10303=CARTESIAN_POINT('Ctrl Pts',(0.600585937444576,2.51434348267211,14.3106180447725));
#10304=CARTESIAN_POINT('Ctrl Pts',(-0.207655199690527,2.44571930558581,
14.3529571514138));
#10305=CARTESIAN_POINT('Ctrl Pts',(-1.01589633682564,2.37709512849952,14.3952962580552));
#10306=CARTESIAN_POINT('Ctrl Pts',(-1.78675514032997,1.86818968138044,14.4376353646965));
#10307=CARTESIAN_POINT('Ctrl Pts',(-2.16743054437203,1.15191511796523,14.4799744713379));
#10308=CARTESIAN_POINT('Ctrl Pts',(-2.3538402493456,0.801168711371672,14.5007071488212));
#10309=CARTESIAN_POINT('Ctrl Pts',(-2.44668866635445,0.400697683916469,
14.5214398263046));
#10310=CARTESIAN_POINT('Ctrl Pts',(-2.44648675330186,0.00013847494270713,
14.542172503788));
#10311=CARTESIAN_POINT('Origin',(0.,0.,0.));
#10312=CARTESIAN_POINT('',(-2.45170362471915,-0.00209312714770177,15.4578274962121));
#10313=CARTESIAN_POINT('',(-2.45101678589125,-0.00220376091521671,15.342172503788));
#10314=CARTESIAN_POINT('',(-2.4505,-3.00099698131059E-16,0.));
#10315=CARTESIAN_POINT('Ctrl Pts',(-2.45170362471915,-0.00209312714770177,
15.4578274962121));
#10316=CARTESIAN_POINT('Ctrl Pts',(-2.44569114235928,0.661629417064826,
15.423287699823));
#10317=CARTESIAN_POINT('Ctrl Pts',(-2.1665957765506,1.32980534203153,15.3887479034339));
#10318=CARTESIAN_POINT('Ctrl Pts',(-1.6855704568615,1.78423176908934,15.3542081070448));
#10319=CARTESIAN_POINT('Ctrl Pts',(-1.09614520521568,2.34106401920079,15.3118847046269));
#10320=CARTESIAN_POINT('Ctrl Pts',(-0.203524735473776,2.57695415849103,
15.2695613022089));
#10321=CARTESIAN_POINT('Ctrl Pts',(0.584040355411103,2.3840150238879,15.2272378997909));
#10322=CARTESIAN_POINT('Ctrl Pts',(1.37160544629598,2.19107588928478,15.184914497373));
#10323=CARTESIAN_POINT('Ctrl Pts',(2.05411515832385,1.56930748078828,15.142591094955));
#10324=CARTESIAN_POINT('Ctrl Pts',(2.31941555059053,0.803082981111423,15.100267692537));
#10325=CARTESIAN_POINT('Ctrl Pts',(2.5847159428572,0.0368584814345732,15.0579442901191));
#10326=CARTESIAN_POINT('Ctrl Pts',(2.43280701536272,-0.873822109422619,
15.0156208877011));
#10327=CARTESIAN_POINT('Ctrl Pts',(1.93316612431206,-1.51244818314025,14.9732974852832));
#10328=CARTESIAN_POINT('Ctrl Pts',(1.43352523326142,-2.15107425685787,14.9309740828652));
#10329=CARTESIAN_POINT('Ctrl Pts',(0.586152378654594,-2.51764581343592,
14.8886506804472));
#10330=CARTESIAN_POINT('Ctrl Pts',(-0.221396377932638,-2.44450698806738,
14.8463272780293));
#10331=CARTESIAN_POINT('Ctrl Pts',(-1.02894513451987,-2.37136816269885,
14.8040038756113));
#10332=CARTESIAN_POINT('Ctrl Pts',(-1.79666979308753,-1.85851895538374,
14.7616804731933));
#10333=CARTESIAN_POINT('Ctrl Pts',(-2.1734423425936,-1.14051705567834,14.7193570707754));
#10334=CARTESIAN_POINT('Ctrl Pts',(-2.35602576259141,-0.792574397475153,
14.6988472125876));
#10335=CARTESIAN_POINT('Ctrl Pts',(-2.44679966025702,-0.39645455782964,
14.6783373543998));
#10336=CARTESIAN_POINT('Ctrl Pts',(-2.44650205703081,-0.000206129442867353,
14.6578274962121));
#10337=CARTESIAN_POINT('Ctrl Pts',(-2.44648675330186,0.00013847494270713,
14.542172503788));
#10338=CARTESIAN_POINT('Ctrl Pts',(-2.44627633088679,-0.417301779901513,
14.5637789329459));
#10339=CARTESIAN_POINT('Ctrl Pts',(-2.34500734273702,-0.834837805473078,
14.5853853621039));
#10340=CARTESIAN_POINT('Ctrl Pts',(-2.14325810848994,-1.19628938140642,
14.6069917912619));
#10341=CARTESIAN_POINT('Ctrl Pts',(-1.74791826398601,-1.90457563765161,
14.6493308979032));
#10342=CARTESIAN_POINT('Ctrl Pts',(-0.96674657039832,-2.39750447043065,
14.6916700045446));
#10343=CARTESIAN_POINT('Ctrl Pts',(-0.157264022288075,-2.44947578697309,
14.7340091111859));
#10344=CARTESIAN_POINT('Ctrl Pts',(0.65221852582217,-2.50144710351553,14.7763482178272));
#10345=CARTESIAN_POINT('Ctrl Pts',(1.49001192845498,-2.11246090382136,14.8186873244686));
#10346=CARTESIAN_POINT('Ctrl Pts',(1.97268097795396,-1.4605455702895,14.8610264311099));
#10347=CARTESIAN_POINT('Ctrl Pts',(2.45535002745294,-0.808630236757634,
14.9033655377512));
#10348=CARTESIAN_POINT('Ctrl Pts',(2.5828947238181,0.106214230611921,14.9457046443926));
#10349=CARTESIAN_POINT('Ctrl Pts',(2.29694133555125,0.865288451737177,14.9880437510339));
#10350=CARTESIAN_POINT('Ctrl Pts',(2.01098794728439,1.62436267286245,15.0303828576753));
#10351=CARTESIAN_POINT('Ctrl Pts',(1.3115364743855,2.22766664774341,15.0727219643166));
#10352=CARTESIAN_POINT('Ctrl Pts',(0.518706793561342,2.39908458916875,15.1150610709579));
#10353=CARTESIAN_POINT('Ctrl Pts',(-0.27412288726279,2.57050253059408,15.1574001775993));
#10354=CARTESIAN_POINT('Ctrl Pts',(-1.16033077601218,2.31003443856381,15.1997392842406));
#10355=CARTESIAN_POINT('Ctrl Pts',(-1.73432367419482,1.73688946015601,15.242078390882));
#10356=CARTESIAN_POINT('Ctrl Pts',(-2.18665025447788,1.28523107046088,15.275443095184));
#10357=CARTESIAN_POINT('Ctrl Pts',(-2.44509151311632,0.639400522100025,
15.308807799486));
#10358=CARTESIAN_POINT('Ctrl Pts',(-2.45101678589125,-0.00220376091521671,
15.342172503788));
#10359=CARTESIAN_POINT('Origin',(0.,0.,0.));
#10360=CARTESIAN_POINT('',(-2.45320425869571,0.00157062206639257,16.2578274962121));
#10361=CARTESIAN_POINT('',(-2.45375743039664,0.00122626908859285,16.142172503788));
#10362=CARTESIAN_POINT('',(-2.4505,-3.00099698131059E-16,0.));
#10363=CARTESIAN_POINT('Ctrl Pts',(-2.45320425869571,0.00157062206639257,
16.2578274962121));
#10364=CARTESIAN_POINT('Ctrl Pts',(-2.45391173395103,0.0963983097870705,
16.2528848500821));
#10365=CARTESIAN_POINT('Ctrl Pts',(-2.44888938633013,0.191150369454898,
16.247942203952));
#10366=CARTESIAN_POINT('Ctrl Pts',(-2.4378864106789,0.285202769094392,16.242999557822));
#10367=CARTESIAN_POINT('Ctrl Pts',(-2.34366899069128,1.09056440203499,16.2006761554041));
#10368=CARTESIAN_POINT('Ctrl Pts',(-1.81093207781014,1.84462463999376,16.1583527529861));
#10369=CARTESIAN_POINT('Ctrl Pts',(-1.08332924046142,2.20250505734567,16.1160293505681));
#10370=CARTESIAN_POINT('Ctrl Pts',(-0.355726403112691,2.56038547469759,
16.0737059481502));
#10371=CARTESIAN_POINT('Ctrl Pts',(0.566742358703627,2.52208607144263,16.0313825457322));
#10372=CARTESIAN_POINT('Ctrl Pts',(1.26217497636144,2.1051235355482,15.9890591433142));
#10373=CARTESIAN_POINT('Ctrl Pts',(1.95760759401923,1.68816099965378,15.9467357408963));
#10374=CARTESIAN_POINT('Ctrl Pts',(2.42600406751854,0.892535331119909,15.9044123384783));
#10375=CARTESIAN_POINT('Ctrl Pts',(2.45313769424733,0.0821354000103284,
15.8620889360604));
#10376=CARTESIAN_POINT('Ctrl Pts',(2.48027132097612,-0.728264531099286,
15.8197655336424));
#10377=CARTESIAN_POINT('Ctrl Pts',(2.06614210093437,-1.55343872478459,15.7774421312244));
#10378=CARTESIAN_POINT('Ctrl Pts',(1.40015696240666,-2.01598394127932,15.7351187288065));
#10379=CARTESIAN_POINT('Ctrl Pts',(0.734171823878979,-2.47852915777403,
15.6927953263885));
#10380=CARTESIAN_POINT('Ctrl Pts',(-0.183669233134644,-2.57844539707816,
15.6504719239706));
#10381=CARTESIAN_POINT('Ctrl Pts',(-0.933580675884534,-2.27003477781442,
15.6081485215526));
#10382=CARTESIAN_POINT('Ctrl Pts',(-1.68349211863445,-1.96162415855066,
15.5658251191346));
#10383=CARTESIAN_POINT('Ctrl Pts',(-2.26547394712063,-1.24488668071899,
15.5235017167167));
#10384=CARTESIAN_POINT('Ctrl Pts',(-2.41334984458884,-0.447630761336837,
15.4811783142987));
#10385=CARTESIAN_POINT('Ctrl Pts',(-2.44054538325779,-0.301009137692811,
15.4733947082698));
#10386=CARTESIAN_POINT('Ctrl Pts',(-2.4530585485704,-0.151664211425061,
15.4656111022409));
#10387=CARTESIAN_POINT('Ctrl Pts',(-2.45170362471915,-0.00209312714770177,
15.4578274962121));
#10388=CARTESIAN_POINT('Ctrl Pts',(-2.45101678589125,-0.00220376091521671,
15.342172503788));
#10389=CARTESIAN_POINT('Ctrl Pts',(-2.45261055940026,-0.174781792067435,
15.3511469061273));
#10390=CARTESIAN_POINT('Ctrl Pts',(-2.43593488648265,-0.347054054347032,
15.3601213084666));
#10391=CARTESIAN_POINT('Ctrl Pts',(-2.39984878306786,-0.515159608355884,
15.369095710806));
#10392=CARTESIAN_POINT('Ctrl Pts',(-2.22960308614234,-1.30824183367466,
15.4114348174473));
#10393=CARTESIAN_POINT('Ctrl Pts',(-1.6273337846754,-2.00858441952683,15.4537739240886));
#10394=CARTESIAN_POINT('Ctrl Pts',(-0.868683124055122,-2.29565965109279,
15.49611303073));
#10395=CARTESIAN_POINT('Ctrl Pts',(-0.110032463434849,-2.58273488265876,
15.5384521373713));
#10396=CARTESIAN_POINT('Ctrl Pts',(0.804999556338751,-2.45654275993851,
15.5807912440127));
#10397=CARTESIAN_POINT('Ctrl Pts',(1.45762771755979,-1.97483797833521,15.623130350654));
#10398=CARTESIAN_POINT('Ctrl Pts',(2.1102558787808,-1.49313319673193,15.6654694572953));
#10399=CARTESIAN_POINT('Ctrl Pts',(2.50048018144927,-0.65591575624562,15.7078085639367));
#10400=CARTESIAN_POINT('Ctrl Pts',(2.44970559717748,0.153642737644857,15.750147670578));
#10401=CARTESIAN_POINT('Ctrl Pts',(2.39893101290568,0.963201231535358,15.7924867772194));
#10402=CARTESIAN_POINT('Ctrl Pts',(1.90715754169359,1.74510077883003,15.8348258838607));
#10403=CARTESIAN_POINT('Ctrl Pts',(1.19945649881003,2.14148726616248,15.877164990502));
#10404=CARTESIAN_POINT('Ctrl Pts',(0.4917554559265,2.53787375349492,15.9195040971434));
#10405=CARTESIAN_POINT('Ctrl Pts',(-0.431873158628486,2.54874718086516,
15.9618432037847));
#10406=CARTESIAN_POINT('Ctrl Pts',(-1.14870970000415,2.16913107690385,16.004182310426));
#10407=CARTESIAN_POINT('Ctrl Pts',(-1.86554624137983,1.78951497294252,16.0465214170674));
#10408=CARTESIAN_POINT('Ctrl Pts',(-2.37559070957618,1.01940933764961,16.0888605237087));
#10409=CARTESIAN_POINT('Ctrl Pts',(-2.44540965195168,0.211270532292635,
16.1311996303501));
#10410=CARTESIAN_POINT('Ctrl Pts',(-2.45144122637565,0.1414563932701,16.1348572548294));
#10411=CARTESIAN_POINT('Ctrl Pts',(-2.45418738704329,0.0713584117786554,
16.1385148793087));
#10412=CARTESIAN_POINT('Ctrl Pts',(-2.45375743039664,0.00122626908859285,
16.142172503788));
#10413=CARTESIAN_POINT('Origin',(0.,0.,0.));
#10414=CARTESIAN_POINT('',(-2.44693273525174,0.00106278712846283,17.0578274962121));
#10415=CARTESIAN_POINT('',(-2.44733932140245,0.00143065932062346,16.942172503788));
#10416=CARTESIAN_POINT('',(-2.4505,-3.00099698131059E-16,0.));
#10417=CARTESIAN_POINT('Ctrl Pts',(-2.44693273525174,0.00106278712846283,
17.0578274962121));
#10418=CARTESIAN_POINT('Ctrl Pts',(-2.44826793617737,0.342274107534463,
17.0401585979232));
#10419=CARTESIAN_POINT('Ctrl Pts',(-2.38175301659422,0.682987849082801,
17.0224896996342));
#10420=CARTESIAN_POINT('Ctrl Pts',(-2.24486236114766,0.992584379473367,
17.0048208013453));
#10421=CARTESIAN_POINT('Ctrl Pts',(-1.91695972664329,1.73418005389911,16.9624973989274));
#10422=CARTESIAN_POINT('Ctrl Pts',(-1.18525817028838,2.29723270973545,16.9201739965094));
#10423=CARTESIAN_POINT('Ctrl Pts',(-0.384410108534635,2.42422351265892,
16.8778505940914));
#10424=CARTESIAN_POINT('Ctrl Pts',(0.416437953219113,2.55121431558239,16.8355271916735));
#10425=CARTESIAN_POINT('Ctrl Pts',(1.28643252037168,2.24214326559299,16.7932037892555));
#10426=CARTESIAN_POINT('Ctrl Pts',(1.82767122184184,1.63836768636443,16.7508803868376));
#10427=CARTESIAN_POINT('Ctrl Pts',(2.36890992331201,1.03459210713585,16.7085569844196));
#10428=CARTESIAN_POINT('Ctrl Pts',(2.58139275909972,0.136111998668031,16.6662335820016));
#10429=CARTESIAN_POINT('Ctrl Pts',(2.36793817501351,-0.646142066565577,
16.6239101795837));
#10430=CARTESIAN_POINT('Ctrl Pts',(2.15448359092731,-1.42839613179916,16.5815867771657));
#10431=CARTESIAN_POINT('Ctrl Pts',(1.51509158696724,-2.09442415379859,16.5392633747478));
#10432=CARTESIAN_POINT('Ctrl Pts',(0.742195707010233,-2.33961028878049,
16.4969399723298));
#10433=CARTESIAN_POINT('Ctrl Pts',(-0.0307001729467758,-2.5847964237624,
16.4546165699118));
#10434=CARTESIAN_POINT('Ctrl Pts',(-0.937099928900703,-2.40914067172678,
16.4122931674939));
#10435=CARTESIAN_POINT('Ctrl Pts',(-1.56245084333064,-1.89298128174774,
16.3699697650759));
#10436=CARTESIAN_POINT('Ctrl Pts',(-2.11477151679402,-1.43710043899317,
16.332589008788));
#10437=CARTESIAN_POINT('Ctrl Pts',(-2.44785369152917,-0.715602040267163,
16.2952082525));
#10438=CARTESIAN_POINT('Ctrl Pts',(-2.45320425869571,0.00157062206639257,
16.2578274962121));
#10439=CARTESIAN_POINT('Ctrl Pts',(-2.45375743039664,0.00122626908859285,
16.142172503788));
#10440=CARTESIAN_POINT('Ctrl Pts',(-2.44921039161454,-0.740461468895879,
16.18085398595));
#10441=CARTESIAN_POINT('Ctrl Pts',(-2.08943753896976,-1.48596989055824,
16.219535468112));
#10442=CARTESIAN_POINT('Ctrl Pts',(-1.50371490001545,-1.93997554189356,
16.2582169502741));
#10443=CARTESIAN_POINT('Ctrl Pts',(-0.862607789149023,-2.4369108353018,
16.3005560569154));
#10444=CARTESIAN_POINT('Ctrl Pts',(0.0491998491384904,-2.58460944669724,
16.3428951635568));
#10445=CARTESIAN_POINT('Ctrl Pts',(0.814398508671991,-2.31547374693528,
16.3852342701981));
#10446=CARTESIAN_POINT('Ctrl Pts',(1.57959716820547,-2.04633804717332,16.4275733768394));
#10447=CARTESIAN_POINT('Ctrl Pts',(2.19818684898495,-1.36036803625397,16.4699124834808));
#10448=CARTESIAN_POINT('Ctrl Pts',(2.387055912797,-0.571513493151793,16.5122515901221));
#10449=CARTESIAN_POINT('Ctrl Pts',(2.57592497660905,0.217341049950412,16.5545906967634));
#10450=CARTESIAN_POINT('Ctrl Pts',(2.33507342345366,1.10908012523546,16.5969298034048));
#10451=CARTESIAN_POINT('Ctrl Pts',(1.77473244518347,1.69557906087766,16.6392689100461));
#10452=CARTESIAN_POINT('Ctrl Pts',(1.21439146691329,2.28207799651985,16.6816080166875));
#10453=CARTESIAN_POINT('Ctrl Pts',(0.334561063528342,2.5633367925192,16.7239471233288));
#10454=CARTESIAN_POINT('Ctrl Pts',(-0.462084367722453,2.41063096320864,
16.7662862299701));
#10455=CARTESIAN_POINT('Ctrl Pts',(-1.25872979897327,2.25792513389807,16.8086253366115));
#10456=CARTESIAN_POINT('Ctrl Pts',(-1.97219025808992,1.67125467927755,16.8509644432528));
#10457=CARTESIAN_POINT('Ctrl Pts',(-2.27593433716645,0.919122677655368,
16.8933035498942));
#10458=CARTESIAN_POINT('Ctrl Pts',(-2.39279757601285,0.629745574349115,
16.9095932011921));
#10459=CARTESIAN_POINT('Ctrl Pts',(-2.449011831938,0.315875736490138,16.92588285249));
#10460=CARTESIAN_POINT('Ctrl Pts',(-2.44733932140245,0.00143065932062346,
16.942172503788));
#10461=CARTESIAN_POINT('Origin',(0.,0.,0.));
#10462=CARTESIAN_POINT('',(-2.44932439460027,-0.00216647677020371,17.8578274962121));
#10463=CARTESIAN_POINT('',(-2.44855018848127,-0.00200161468709733,17.742172503788));
#10464=CARTESIAN_POINT('',(-2.4505,-3.00099698131059E-16,0.));
#10465=CARTESIAN_POINT('Ctrl Pts',(-2.44932439460027,-0.00216647677020371,
17.8578274962121));
#10466=CARTESIAN_POINT('Ctrl Pts',(-2.44432735118055,0.583364483646701,
17.8274323457643));
#10467=CARTESIAN_POINT('Ctrl Pts',(-2.23380041902901,1.17212217287416,17.7970371953165));
#10468=CARTESIAN_POINT('Ctrl Pts',(-1.85150344977178,1.61138628092558,17.7666420448687));
#10469=CARTESIAN_POINT('Ctrl Pts',(-1.31917812041283,2.22303489390921,17.7243186424507));
#10470=CARTESIAN_POINT('Ctrl Pts',(-0.453810057673014,2.54483230969522,
17.6819952400327));
#10471=CARTESIAN_POINT('Ctrl Pts',(0.348814354230171,2.42960064972722,17.6396718376148));
#10472=CARTESIAN_POINT('Ctrl Pts',(1.15143876613336,2.31436898975923,17.5973484351968));
#10473=CARTESIAN_POINT('Ctrl Pts',(1.89131952719991,1.76210825403724,17.5550250327788));
#10474=CARTESIAN_POINT('Ctrl Pts',(2.23006336434382,1.02540146376113,17.5127016303609));
#10475=CARTESIAN_POINT('Ctrl Pts',(2.56880720148773,0.288694673485041,17.4703782279429));
#10476=CARTESIAN_POINT('Ctrl Pts',(2.50641411470901,-0.632458171345165,
17.428054825525));
#10477=CARTESIAN_POINT('Ctrl Pts',(2.07142032492868,-1.31675685240075,17.385731423107));
#10478=CARTESIAN_POINT('Ctrl Pts',(1.63642653514833,-2.00105553345636,17.343408020689));
#10479=CARTESIAN_POINT('Ctrl Pts',(0.828832042366333,-2.44850005073733,
17.3010846182711));
#10480=CARTESIAN_POINT('Ctrl Pts',(0.0179998008846638,-2.45444632820522,
17.2587612158531));
#10481=CARTESIAN_POINT('Ctrl Pts',(-0.792832440596982,-2.4603926056731,
17.2164378134351));
#10482=CARTESIAN_POINT('Ctrl Pts',(-1.6069024307783,-2.02484064332792,17.1741144110172));
#10483=CARTESIAN_POINT('Ctrl Pts',(-2.05188556954207,-1.34699531564776,
17.1317910085992));
#10484=CARTESIAN_POINT('Ctrl Pts',(-2.31110004676363,-0.95213243895576,
17.1071365044702));
#10485=CARTESIAN_POINT('Ctrl Pts',(-2.44506964700506,-0.475050424361855,
17.0824820003411));
#10486=CARTESIAN_POINT('Ctrl Pts',(-2.44693273525174,0.00106278712846283,
17.0578274962121));
#10487=CARTESIAN_POINT('Ctrl Pts',(-2.44733932140245,0.00143065932062346,
16.942172503788));
#10488=CARTESIAN_POINT('Ctrl Pts',(-2.44466474060817,-0.501411473139033,
16.9682219591314));
#10489=CARTESIAN_POINT('Ctrl Pts',(-2.29395904503527,-1.00572463812667,
16.9942714144748));
#10490=CARTESIAN_POINT('Ctrl Pts',(-2.00651806831996,-1.41370040856583,
17.0203208698182));
#10491=CARTESIAN_POINT('Ctrl Pts',(-1.53933002136053,-2.07679794454109,
17.0626599764595));
#10492=CARTESIAN_POINT('Ctrl Pts',(-0.710926228405238,-2.48539946786777,
17.1049990831009));
#10493=CARTESIAN_POINT('Ctrl Pts',(0.0995554713400155,-2.45249919710485,
17.1473381897422));
#10494=CARTESIAN_POINT('Ctrl Pts',(0.910037171085223,-2.41959892634193,
17.1896772963835));
#10495=CARTESIAN_POINT('Ctrl Pts',(1.7025967776204,-1.94519686148946,17.2320164030249));
#10496=CARTESIAN_POINT('Ctrl Pts',(2.11450135898779,-1.24641389855554,17.2743555096662));
#10497=CARTESIAN_POINT('Ctrl Pts',(2.52640594035523,-0.547630935621566,
17.3166946163075));
#10498=CARTESIAN_POINT('Ctrl Pts',(2.55765549655481,0.375532925393901,17.3590337229489));
#10499=CARTESIAN_POINT('Ctrl Pts',(2.19394795737102,1.10057074466896,17.4013728295902));
#10500=CARTESIAN_POINT('Ctrl Pts',(1.83024041818725,1.82560856394398,17.4437119362316));
#10501=CARTESIAN_POINT('Ctrl Pts',(1.07157578362015,2.35252034147863,17.4860510428729));
#10502=CARTESIAN_POINT('Ctrl Pts',(0.265174180711339,2.44015291683897,17.5283901495142));
#10503=CARTESIAN_POINT('Ctrl Pts',(-0.541227422197499,2.52778549219932,
17.5707292561556));
#10504=CARTESIAN_POINT('Ctrl Pts',(-1.39536599344806,2.17613886538534,17.6130683627969));
#10505=CARTESIAN_POINT('Ctrl Pts',(-1.90632558716922,1.54615211391946,17.6554074694383));
#10506=CARTESIAN_POINT('Ctrl Pts',(-2.25536008677173,1.11581062849447,17.6843291475548));
#10507=CARTESIAN_POINT('Ctrl Pts',(-2.44426032078067,0.555590000217446,
17.7132508256714));
#10508=CARTESIAN_POINT('Ctrl Pts',(-2.44855018848127,-0.00200161468709733,
17.742172503788));
#10509=CARTESIAN_POINT('Origin',(0.,0.,0.));
#10510=CARTESIAN_POINT('',(-2.45447131381915,0.000284333535872242,18.6578274962121));
#10511=CARTESIAN_POINT('',(-2.45447923121619,-0.000280315077781223,18.542172503788));
#10512=CARTESIAN_POINT('',(-2.4505,-3.00099698131059E-16,0.));
#10513=CARTESIAN_POINT('Ctrl Pts',(-2.45447131381915,0.000284333535872242,
18.6578274962121));
#10514=CARTESIAN_POINT('Ctrl Pts',(-2.45449642498564,0.0155735304685792,
18.6570294960233));
#10515=CARTESIAN_POINT('Ctrl Pts',(-2.45436591171342,0.0308622871987328,
18.6562314958346));
#10516=CARTESIAN_POINT('Ctrl Pts',(-2.45407846744843,0.0461480928960939,
18.6554334956459));
#10517=CARTESIAN_POINT('Ctrl Pts',(-2.43883333408655,0.856858810692927,
18.6131100932279));
#10518=CARTESIAN_POINT('Ctrl Pts',(-1.98215613057064,1.65926855178873,18.5707866908099));
#10519=CARTESIAN_POINT('Ctrl Pts',(-1.29291361188798,2.08638566978081,18.528463288392));
#10520=CARTESIAN_POINT('Ctrl Pts',(-0.603671093205304,2.51350278777291,
18.486139885974));
#10521=CARTESIAN_POINT('Ctrl Pts',(0.318136740644127,2.56532728266126,18.443816483556));
#10522=CARTESIAN_POINT('Ctrl Pts',(1.0509101043071,2.2181566048269,18.4014930811381));
#10523=CARTESIAN_POINT('Ctrl Pts',(1.78368346797003,1.87098592699256,18.3591696787201));
#10524=CARTESIAN_POINT('Ctrl Pts',(2.32742236144652,1.12482007643556,18.3168462763022));
#10525=CARTESIAN_POINT('Ctrl Pts',(2.43344132952563,0.320926886733544,18.2745228738842));
#10526=CARTESIAN_POINT('Ctrl Pts',(2.53946029760475,-0.482966302968517,
18.2321994714662));
#10527=CARTESIAN_POINT('Ctrl Pts',(2.20775934028643,-1.3445868318156,18.1898760690483));
#10528=CARTESIAN_POINT('Ctrl Pts',(1.59004583873153,-1.86986229482401,18.1475526666303));
#10529=CARTESIAN_POINT('Ctrl Pts',(0.972332337176633,-2.39513775783242,
18.1052292642124));
#10530=CARTESIAN_POINT('Ctrl Pts',(0.0686062913851572,-2.58406815500216,
18.0629058617944));
#10531=CARTESIAN_POINT('Ctrl Pts',(-0.707802434290682,-2.35024392029511,
18.0205824593764));
#10532=CARTESIAN_POINT('Ctrl Pts',(-1.4842111599665,-2.11641968558808,17.9782590569585));
#10533=CARTESIAN_POINT('Ctrl Pts',(-2.13330256552669,-1.45984081900429,
17.9359356545405));
#10534=CARTESIAN_POINT('Ctrl Pts',(-2.35820697031774,-0.680801480621775,
17.8936122521225));
#10535=CARTESIAN_POINT('Ctrl Pts',(-2.42159309374546,-0.46124026880983,
17.8816840001524));
#10536=CARTESIAN_POINT('Ctrl Pts',(-2.45128543088856,-0.231951844806988,
17.8697557481822));
#10537=CARTESIAN_POINT('Ctrl Pts',(-2.44932439460027,-0.00216647677020371,
17.8578274962121));
#10538=CARTESIAN_POINT('Ctrl Pts',(-2.44855018848127,-0.00200161468709733,
17.742172503788));
#10539=CARTESIAN_POINT('Ctrl Pts',(-2.45054035630699,-0.260681128677846,
17.7555899323127));
#10540=CARTESIAN_POINT('Ctrl Pts',(-2.41279785980027,-0.518794814714601,
17.7690073608375));
#10541=CARTESIAN_POINT('Ctrl Pts',(-2.33287882030774,-0.763112058241259,
17.7824247893623));
#10542=CARTESIAN_POINT('Ctrl Pts',(-2.08069184353337,-1.53406260281827,
17.8247638960036));
#10543=CARTESIAN_POINT('Ctrl Pts',(-1.40853727379288,-2.16763681585453,
17.867103002645));
#10544=CARTESIAN_POINT('Ctrl Pts',(-0.624041939151175,-2.37386504710232,
17.9094421092863));
#10545=CARTESIAN_POINT('Ctrl Pts',(0.160453395490553,-2.58009327835011,
17.9517812159276));
#10546=CARTESIAN_POINT('Ctrl Pts',(1.0572894950335,-2.35897552780941,17.994120322569));
#10547=CARTESIAN_POINT('Ctrl Pts',(1.65600891856045,-1.81171136368957,18.0364594292103));
#10548=CARTESIAN_POINT('Ctrl Pts',(2.25472834208738,-1.26444719956974,18.0787985358516));
#10549=CARTESIAN_POINT('Ctrl Pts',(2.55533108959832,-0.39103662187079,18.121137642493));
#10550=CARTESIAN_POINT('Ctrl Pts',(2.420239476008,0.408784151412672,18.1634767491343));
#10551=CARTESIAN_POINT('Ctrl Pts',(2.28514786241768,1.20860492469616,18.2058158557757));
#10552=CARTESIAN_POINT('Ctrl Pts',(1.71436188772607,1.93483589356415,18.248154962417));
#10553=CARTESIAN_POINT('Ctrl Pts',(0.969114736684281,2.25510093583747,18.2904940690583));
#10554=CARTESIAN_POINT('Ctrl Pts',(0.223867585642514,2.57536597811077,18.3328331756997));
#10555=CARTESIAN_POINT('Ctrl Pts',(-0.695840741749422,2.48966509378942,
18.375172282341));
#10556=CARTESIAN_POINT('Ctrl Pts',(-1.36908480923408,2.03722124198579,18.4175113889823));
#10557=CARTESIAN_POINT('Ctrl Pts',(-2.02984001993379,1.59317034415132,18.4590650939176));
#10558=CARTESIAN_POINT('Ctrl Pts',(-2.45319011466729,0.795856637511719,
18.5006187988528));
#10559=CARTESIAN_POINT('Ctrl Pts',(-2.45447923121619,-0.000280315077781223,
18.542172503788));
#10560=CARTESIAN_POINT('Origin',(0.,0.,0.));
#10561=CARTESIAN_POINT('',(-2.44849865710204,0.00198121704041709,19.4578274962121));
#10562=CARTESIAN_POINT('',(-2.44936952853288,0.00217752272054485,19.342172503788));
#10563=CARTESIAN_POINT('',(-2.4505,-3.00099698131059E-16,0.));
#10564=CARTESIAN_POINT('Ctrl Pts',(-2.44849865710204,0.00198121704041709,
19.4578274962121));
#10565=CARTESIAN_POINT('Ctrl Pts',(-2.45048258357382,0.262734228461402,
19.4443032438644));
#10566=CARTESIAN_POINT('Ctrl Pts',(-2.412119819907,0.522918749126386,19.4307789915168));
#10567=CARTESIAN_POINT('Ctrl Pts',(-2.33094434568626,0.768979341845459,
19.4172547391692));
#10568=CARTESIAN_POINT('Ctrl Pts',(-2.07691017258718,1.53901240668088,19.3749313367512));
#10569=CARTESIAN_POINT('Ctrl Pts',(-1.40359291560209,2.17072383784431,19.3326079343333));
#10570=CARTESIAN_POINT('Ctrl Pts',(-0.618942236900824,2.37519289285147,
19.2902845319153));
#10571=CARTESIAN_POINT('Ctrl Pts',(0.165708441800439,2.57966194785863,19.2479611294973));
#10572=CARTESIAN_POINT('Ctrl Pts',(1.06169254221783,2.35688862670957,19.2056377270794));
#10573=CARTESIAN_POINT('Ctrl Pts',(1.6592210708706,1.80876095956626,19.1633143246614));
#10574=CARTESIAN_POINT('Ctrl Pts',(2.25674959952335,1.26063329242296,19.1209909222434));
#10575=CARTESIAN_POINT('Ctrl Pts',(2.55582255641143,0.387151279285426,19.0786675198255));
#10576=CARTESIAN_POINT('Ctrl Pts',(2.41965536475122,-0.41218768383175,19.0363441174075));
#10577=CARTESIAN_POINT('Ctrl Pts',(2.283488173091,-1.21152664694893,18.9940207149896));
#10578=CARTESIAN_POINT('Ctrl Pts',(1.71208083288248,-1.93672256004577,18.9516973125716));
#10579=CARTESIAN_POINT('Ctrl Pts',(0.966773292794929,-2.25609844005318,
18.9093739101536));
#10580=CARTESIAN_POINT('Ctrl Pts',(0.221465752707379,-2.57547432006059,
18.8670505077357));
#10581=CARTESIAN_POINT('Ctrl Pts',(-0.697741987259225,-2.48903016697857,
18.8247271053177));
#10582=CARTESIAN_POINT('Ctrl Pts',(-1.37043932563863,-2.03630224318865,
18.7824037028997));
#10583=CARTESIAN_POINT('Ctrl Pts',(-2.03045307592447,-1.59211042349219,
18.7408783006705));
#10584=CARTESIAN_POINT('Ctrl Pts',(-2.45316460825219,-0.795317047709615,
18.6993528984413));
#10585=CARTESIAN_POINT('Ctrl Pts',(-2.45447131381915,0.000284333535872242,
18.6578274962121));
#10586=CARTESIAN_POINT('Ctrl Pts',(-2.45447923121619,-0.000280315077781223,
18.542172503788));
#10587=CARTESIAN_POINT('Ctrl Pts',(-2.45450359665697,-0.0153280062970204,
18.5429579054941));
#10588=CARTESIAN_POINT('Ctrl Pts',(-2.45437718361159,-0.030375277128677,
18.5437433072002));
#10589=CARTESIAN_POINT('Ctrl Pts',(-2.45409874524395,-0.0454197343205972,
18.5445287089064));
#10590=CARTESIAN_POINT('Ctrl Pts',(-2.43908880619174,-0.856430039537394,
18.5868678155477));
#10591=CARTESIAN_POINT('Ctrl Pts',(-1.98228912050995,-1.65926383068508,
18.629206922189));
#10592=CARTESIAN_POINT('Ctrl Pts',(-1.29276445498518,-2.08648596151533,
18.6715460288304));
#10593=CARTESIAN_POINT('Ctrl Pts',(-0.603239789460381,-2.51370809234559,
18.7138851354717));
#10594=CARTESIAN_POINT('Ctrl Pts',(0.319009855907422,-2.56531856285839,
18.7562242421131));
#10595=CARTESIAN_POINT('Ctrl Pts',(1.0518959528828,-2.21769666726143,18.7985633487544));
#10596=CARTESIAN_POINT('Ctrl Pts',(1.78478204985816,-1.87007477166448,18.8409024553957));
#10597=CARTESIAN_POINT('Ctrl Pts',(2.32830459844111,-1.12322050995779,18.8832415620371));
#10598=CARTESIAN_POINT('Ctrl Pts',(2.4337081409891,-0.318948723397725,18.9255806686784));
#10599=CARTESIAN_POINT('Ctrl Pts',(2.5391116835371,0.485323063162368,18.9679197753197));
#10600=CARTESIAN_POINT('Ctrl Pts',(2.20639622005011,1.34701237457585,19.0102588819611));
#10601=CARTESIAN_POINT('Ctrl Pts',(1.58783655053459,1.87174749698245,19.0525979886024));
#10602=CARTESIAN_POINT('Ctrl Pts',(0.969276881019064,2.39648261938906,19.0949370952438));
#10603=CARTESIAN_POINT('Ctrl Pts',(0.0648730054750031,2.58426355278879,
19.1372762018851));
#10604=CARTESIAN_POINT('Ctrl Pts',(-0.711454070352378,2.3491480816357,19.1796153085265));
#10605=CARTESIAN_POINT('Ctrl Pts',(-1.48778114617976,2.11403261048261,19.2219544151678));
#10606=CARTESIAN_POINT('Ctrl Pts',(-2.13603142229046,1.45602073477671,19.2642935218091));
#10607=CARTESIAN_POINT('Ctrl Pts',(-2.35951841434036,0.676266556959933,
19.3066326284505));
#10608=CARTESIAN_POINT('Ctrl Pts',(-2.42205082993341,0.458088703025711,
19.318479253563));
#10609=CARTESIAN_POINT('Ctrl Pts',(-2.45132855731013,0.230379652654894,
19.3303258786755));
#10610=CARTESIAN_POINT('Ctrl Pts',(-2.44936952853288,0.00217752272054485,
19.342172503788));
#10611=CARTESIAN_POINT('Origin',(0.,0.,0.));
#10612=CARTESIAN_POINT('',(-2.4474177661784,-0.00147899005716184,20.2578274962121));
#10613=CARTESIAN_POINT('',(-2.44688139258877,-0.00101268112437026,20.142172503788));
#10614=CARTESIAN_POINT('',(-2.4505,-3.00099698131059E-16,0.));
#10615=CARTESIAN_POINT('Ctrl Pts',(-2.4474177661784,-0.00147899005716184,
20.2578274962121));
#10616=CARTESIAN_POINT('Ctrl Pts',(-2.4446244023887,0.505203710649909,20.2315769917055));
#10617=CARTESIAN_POINT('Ctrl Pts',(-2.29139905917431,1.01343507544043,20.205326487199));
#10618=CARTESIAN_POINT('Ctrl Pts',(-1.99979327751963,1.42318572858794,20.1790759826925));
#10619=CARTESIAN_POINT('Ctrl Pts',(-1.52964045278787,2.08382224244525,20.1367525802745));
#10620=CARTESIAN_POINT('Ctrl Pts',(-0.699770977560138,2.48846049433743,
20.0944291778566));
#10621=CARTESIAN_POINT('Ctrl Pts',(0.110264465500261,2.45203436324133,20.0521057754386));
#10622=CARTESIAN_POINT('Ctrl Pts',(0.920299908560683,2.41560823214523,20.0097823730206));
#10623=CARTESIAN_POINT('Ctrl Pts',(1.71050131945374,1.93811771806081,19.9674589706027));
#10624=CARTESIAN_POINT('Ctrl Pts',(2.11946067691125,1.23794879130831,19.9251355681847));
#10625=CARTESIAN_POINT('Ctrl Pts',(2.52842003436875,0.537779864555827,19.8828121657668));
#10626=CARTESIAN_POINT('Ctrl Pts',(2.55613733839068,-0.385067474864773,
19.8404887633488));
#10627=CARTESIAN_POINT('Ctrl Pts',(2.18993575005719,-1.10851801135245,19.7981653609308));
#10628=CARTESIAN_POINT('Ctrl Pts',(1.8237341617237,-1.83196854784013,19.7558419585129));
#10629=CARTESIAN_POINT('Ctrl Pts',(1.06361368103481,-2.35602228139494,19.7135185560949));
#10630=CARTESIAN_POINT('Ctrl Pts',(0.257224457764118,-2.44099699901485,
19.6711951536769));
#10631=CARTESIAN_POINT('Ctrl Pts',(-0.549164765506549,-2.52597171663476,
19.628871751259));
#10632=CARTESIAN_POINT('Ctrl Pts',(-1.40182273135899,-2.17186741831979,
19.586548348841));
#10633=CARTESIAN_POINT('Ctrl Pts',(-1.91077616967869,-1.54063791990863,
19.5442249464231));
#10634=CARTESIAN_POINT('Ctrl Pts',(-2.25709583236163,-1.11111496062379,
19.5154257963527));
#10635=CARTESIAN_POINT('Ctrl Pts',(-2.44427399501199,-0.553277951021609,
19.4866266462824));
#10636=CARTESIAN_POINT('Ctrl Pts',(-2.44849865710204,0.00198121704041709,
19.4578274962121));
#10637=CARTESIAN_POINT('Ctrl Pts',(-2.44936952853288,0.00217752272054485,
19.342172503788));
#10638=CARTESIAN_POINT('Ctrl Pts',(-2.44432710942723,-0.585200668602821,
19.3726649853168));
#10639=CARTESIAN_POINT('Ctrl Pts',(-2.23233624155838,-1.1758455900017,19.4031574668456));
#10640=CARTESIAN_POINT('Ctrl Pts',(-1.84780821169541,-1.61563251281492,
19.4336499483745));
#10641=CARTESIAN_POINT('Ctrl Pts',(-1.31388730901146,-2.2262809248454,19.4759890550158));
#10642=CARTESIAN_POINT('Ctrl Pts',(-0.447321795654437,-2.54608126897873,
19.5183281616572));
#10643=CARTESIAN_POINT('Ctrl Pts',(0.355284909779008,-2.42866964335559,
19.5606672682985));
#10644=CARTESIAN_POINT('Ctrl Pts',(1.15789161521248,-2.31125801773245,19.6030063749398));
#10645=CARTESIAN_POINT('Ctrl Pts',(1.89653951272237,-1.75663442235281,19.6453454815812));
#10646=CARTESIAN_POINT('Ctrl Pts',(2.23316959029373,-1.01863496143666,19.6876845882225));
#10647=CARTESIAN_POINT('Ctrl Pts',(2.56979966786507,-0.280635500520529,
19.7300236948639));
#10648=CARTESIAN_POINT('Ctrl Pts',(2.50441192549792,0.640739825932114,19.7723628015052));
#10649=CARTESIAN_POINT('Ctrl Pts',(2.06693255083469,1.3238026416251,19.8147019081465));
#10650=CARTESIAN_POINT('Ctrl Pts',(1.62945317617146,2.00686545731811,19.8570410147879));
#10651=CARTESIAN_POINT('Ctrl Pts',(0.819882169212132,2.45161576225146,19.8993801214292));
#10652=CARTESIAN_POINT('Ctrl Pts',(0.00873811626980386,2.45450346282045,
19.9417192280705));
#10653=CARTESIAN_POINT('Ctrl Pts',(-0.802405936672501,2.45739116338945,
19.9840583347119));
#10654=CARTESIAN_POINT('Ctrl Pts',(-1.61512303559781,2.01841625959413,20.0263974413532));
#10655=CARTESIAN_POINT('Ctrl Pts',(-2.05745471364159,1.33848560133759,20.0687365479946));
#10656=CARTESIAN_POINT('Ctrl Pts',(-2.31319188062225,0.945378914846541,
20.0932151999257));
#10657=CARTESIAN_POINT('Ctrl Pts',(-2.44512196288412,0.471729021673493,
20.1176938518568));
#10658=CARTESIAN_POINT('Ctrl Pts',(-2.44688139258877,-0.00101268112437026,
20.142172503788));
#10659=CARTESIAN_POINT('Origin',(0.,0.,0.));
#10660=CARTESIAN_POINT('',(-2.45386624914882,-0.00113190329454754,21.0578274962121));
#10661=CARTESIAN_POINT('',(-2.45307396903907,-0.00164186243163431,20.9421725037879));
#10662=CARTESIAN_POINT('',(-2.4505,-3.00099698131059E-16,0.));
#10663=CARTESIAN_POINT('Ctrl Pts',(-2.45386624914882,-0.00113190329454754,
21.0578274962121));
#10664=CARTESIAN_POINT('Ctrl Pts',(-2.4495767373451,0.74612978248249,21.0188507395466));
#10665=CARTESIAN_POINT('Ctrl Pts',(-2.08354403586559,1.49702756493175,20.9798739828812));
#10666=CARTESIAN_POINT('Ctrl Pts',(-1.49017767759624,1.95038490049398,20.9408972262158));
#10667=CARTESIAN_POINT('Ctrl Pts',(-0.845863339748866,2.44266867661335,
20.8985738237978));
#10668=CARTESIAN_POINT('Ctrl Pts',(0.0664995651392659,2.58412322862684,
20.8562504213799));
#10669=CARTESIAN_POINT('Ctrl Pts',(0.829631002671575,2.31005263361174,20.8139270189619));
#10670=CARTESIAN_POINT('Ctrl Pts',(1.59276244020384,2.03598203859666,20.771603616544));
#10671=CARTESIAN_POINT('Ctrl Pts',(2.2066624103803,1.34638629655305,20.729280214126));
#10672=CARTESIAN_POINT('Ctrl Pts',(2.39055645427188,0.556660228447093,20.686956811708));
#10673=CARTESIAN_POINT('Ctrl Pts',(2.57445049816346,-0.233065839658858,
20.6446334092901));
#10674=CARTESIAN_POINT('Ctrl Pts',(2.32833861577016,-1.12292223382715,20.6023100068721));
#10675=CARTESIAN_POINT('Ctrl Pts',(1.76478300611921,-1.7059225399107,20.5599866044542));
#10676=CARTESIAN_POINT('Ctrl Pts',(1.20122739646826,-2.28892284599426,20.5176632020362));
#10677=CARTESIAN_POINT('Ctrl Pts',(0.320228059559642,-2.56506706399307,
20.4753397996182));
#10678=CARTESIAN_POINT('Ctrl Pts',(-0.47527947112366,-2.40805734881286,
20.4330163972002));
#10679=CARTESIAN_POINT('Ctrl Pts',(-1.27078700180694,-2.25104763363266,
20.3906929947823));
#10680=CARTESIAN_POINT('Ctrl Pts',(-1.98080272626491,-1.66088398527347,
20.3483695923644));
#10681=CARTESIAN_POINT('Ctrl Pts',(-2.28059250137602,-0.907484773182661,
20.3060461899464));
#10682=CARTESIAN_POINT('Ctrl Pts',(-2.39444181818354,-0.62137099379153,
20.289973292035));
#10683=CARTESIAN_POINT('Ctrl Pts',(-2.44912811239328,-0.311715287417987,
20.2739003941235));
#10684=CARTESIAN_POINT('Ctrl Pts',(-2.4474177661784,-0.00147899005716184,
20.2578274962121));
#10685=CARTESIAN_POINT('Ctrl Pts',(-2.44688139258877,-0.00101268112437026,
20.142172503788));
#10686=CARTESIAN_POINT('Ctrl Pts',(-2.44816513217721,-0.345941061829376,
20.1600329584982));
#10687=CARTESIAN_POINT('Ctrl Pts',(-2.38015048719084,-0.690385953171378,
20.1778934132084));
#10688=CARTESIAN_POINT('Ctrl Pts',(-2.24036564400662,-1.00270902301118,
20.1957538679186));
#10689=CARTESIAN_POINT('Ctrl Pts',(-1.9089986391656,-1.74308657638562,20.2380929745599));
#10690=CARTESIAN_POINT('Ctrl Pts',(-1.17431837232131,-2.30295527041674,
20.2804320812012));
#10691=CARTESIAN_POINT('Ctrl Pts',(-0.372567979063618,-2.42607846217914,
20.3227711878426));
#10692=CARTESIAN_POINT('Ctrl Pts',(0.429182414194054,-2.54920165394154,
20.3651102944839));
#10693=CARTESIAN_POINT('Ctrl Pts',(1.29800293386513,-2.23557934343526,20.4074494011253));
#10694=CARTESIAN_POINT('Ctrl Pts',(1.83625810641794,-1.62874791489994,20.4497885077666));
#10695=CARTESIAN_POINT('Ctrl Pts',(2.37451327897076,-1.02191648636461,20.492127614408));
#10696=CARTESIAN_POINT('Ctrl Pts',(2.58220310440529,-0.121875939800231,
20.5344667210493));
#10697=CARTESIAN_POINT('Ctrl Pts',(2.3642736098797,0.659449695804327,20.5768058276906));
#10698=CARTESIAN_POINT('Ctrl Pts',(2.14634411535412,1.44077533140884,20.619144934332));
#10699=CARTESIAN_POINT('Ctrl Pts',(1.50279530086847,2.10338605605354,20.6614840409733));
#10700=CARTESIAN_POINT('Ctrl Pts',(0.72816191990582,2.34402299947547,20.7038231476146));
#10701=CARTESIAN_POINT('Ctrl Pts',(-0.0464714610568923,2.58465994289741,
20.746162254256));
#10702=CARTESIAN_POINT('Ctrl Pts',(-0.95218940849662,2.40332310509649,20.7885013608973));
#10703=CARTESIAN_POINT('Ctrl Pts',(-1.57446950176282,1.88300541467923,20.8308404675387));
#10704=CARTESIAN_POINT('Ctrl Pts',(-2.11990464353851,1.42694140698852,20.8679511462884));
#10705=CARTESIAN_POINT('Ctrl Pts',(-2.44758271427281,0.710448255773275,
20.9050618250382));
#10706=CARTESIAN_POINT('Ctrl Pts',(-2.45307396903907,-0.00164186243163431,
20.9421725037879));
#10707=CARTESIAN_POINT('Origin',(0.,0.,0.));
#10708=CARTESIAN_POINT('',(-2.45077715073522,0.00222010580503924,21.857827496212));
#10709=CARTESIAN_POINT('',(-2.45192339561065,0.00204828064707867,21.7421725037879));
#10710=CARTESIAN_POINT('',(-2.4505,-3.00099698131059E-16,0.));
#10711=CARTESIAN_POINT('Ctrl Pts',(-2.45077715073522,0.00222010580503924,
21.857827496212));
#10712=CARTESIAN_POINT('Ctrl Pts',(-2.45244026375057,0.182635521438812,
21.8484478898057));
#10713=CARTESIAN_POINT('Ctrl Pts',(-2.43420592996322,0.362717763180709,
21.8390682833993));
#10714=CARTESIAN_POINT('Ctrl Pts',(-2.39481453108522,0.538046615944328,
21.829688676993));
#10715=CARTESIAN_POINT('Ctrl Pts',(-2.21706954325802,1.32917934257705,21.787365274575));
#10716=CARTESIAN_POINT('Ctrl Pts',(-1.6085526804466,2.02352991753004,21.7450418721571));
#10717=CARTESIAN_POINT('Ctrl Pts',(-0.847576397798938,2.30352882078366,
21.7027184697391));
#10718=CARTESIAN_POINT('Ctrl Pts',(-0.0866001151512351,2.5835277240373,
21.6603950673212));
#10719=CARTESIAN_POINT('Ctrl Pts',(0.826835587332673,2.44917495559155,21.6180716649032));
#10720=CARTESIAN_POINT('Ctrl Pts',(1.47496003114712,1.96191836357903,21.5757482624852));
#10721=CARTESIAN_POINT('Ctrl Pts',(2.12308447496153,1.47466177156653,21.5334248600673));
#10722=CARTESIAN_POINT('Ctrl Pts',(2.50589766010645,0.634501355987238,21.4911014576493));
#10723=CARTESIAN_POINT('Ctrl Pts',(2.44831541284178,-0.174305521802888,
21.4487780552313));
#10724=CARTESIAN_POINT('Ctrl Pts',(2.39073316557711,-0.983112399593038,
21.4064546528134));
#10725=CARTESIAN_POINT('Ctrl Pts',(1.89275548590292,-1.76056573959403,21.3641312503954));
#10726=CARTESIAN_POINT('Ctrl Pts',(1.18213839674829,-2.15108799968291,21.3218078479775));
#10727=CARTESIAN_POINT('Ctrl Pts',(0.471521307593673,-2.54161025977178,
21.2794844455595));
#10728=CARTESIAN_POINT('Ctrl Pts',(-0.451735191041368,-2.54520143994851,
21.2371610431415));
#10729=CARTESIAN_POINT('Ctrl Pts',(-1.16536875158895,-2.16021907269529,
21.1948376407236));
#10730=CARTESIAN_POINT('Ctrl Pts',(-1.87900231213655,-1.77523670544206,
21.1525142383056));
#10731=CARTESIAN_POINT('Ctrl Pts',(-2.38301293459671,-1.00168079075884,
21.1101908358877));
#10732=CARTESIAN_POINT('Ctrl Pts',(-2.44688536042345,-0.193346333304644,
21.0678674334697));
#10733=CARTESIAN_POINT('Ctrl Pts',(-2.45193595584786,-0.1294287623126,21.0645207877171));
#10734=CARTESIAN_POINT('Ctrl Pts',(-2.45423455779445,-0.0652937361585034,
21.0611741419646));
#10735=CARTESIAN_POINT('Ctrl Pts',(-2.45386624914882,-0.00113190329454754,
21.0578274962121));
#10736=CARTESIAN_POINT('Ctrl Pts',(-2.45307396903907,-0.00164186243163431,
20.9421725037879));
#10737=CARTESIAN_POINT('Ctrl Pts',(-2.45384761777164,-0.101966404066716,
20.9474009316795));
#10738=CARTESIAN_POINT('Ctrl Pts',(-2.44822609471337,-0.202203548728654,
20.9526293595711));
#10739=CARTESIAN_POINT('Ctrl Pts',(-2.43591736083732,-0.301612690077846,
20.9578577874627));
#10740=CARTESIAN_POINT('Ctrl Pts',(-2.33624288755297,-1.10661456138417,
21.000196894104));
#10741=CARTESIAN_POINT('Ctrl Pts',(-1.79805170189159,-1.85731976096327,
21.0425360007454));
#10742=CARTESIAN_POINT('Ctrl Pts',(-1.06765924194229,-2.2101509782728,21.0848751073867));
#10743=CARTESIAN_POINT('Ctrl Pts',(-0.337266781992992,-2.56298219558234,
21.127214214028));
#10744=CARTESIAN_POINT('Ctrl Pts',(0.585326952244219,-2.51793943062228,
21.1695533206693));
#10745=CARTESIAN_POINT('Ctrl Pts',(1.27787595235591,-2.09563752929443,21.2118924273107));
#10746=CARTESIAN_POINT('Ctrl Pts',(1.97042495246761,-1.67333562796657,21.254231533952));
#10747=CARTESIAN_POINT('Ctrl Pts',(2.43292921845375,-0.873774590270887,
21.2965706405934));
#10748=CARTESIAN_POINT('Ctrl Pts',(2.45371315274431,-0.0628917124923539,
21.3389097472348));
#10749=CARTESIAN_POINT('Ctrl Pts',(2.47449708703488,0.747991165286156,21.3812488538761));
#10750=CARTESIAN_POINT('Ctrl Pts',(2.05356068962983,1.57019588314754,21.4235879605174));
#10751=CARTESIAN_POINT('Ctrl Pts',(1.38355507737789,2.02742174979691,21.4659270671587));
#10752=CARTESIAN_POINT('Ctrl Pts',(0.713549465125928,2.48464761644628,21.5082661738001));
#10753=CARTESIAN_POINT('Ctrl Pts',(-0.20552536197295,2.57689463188366,21.5506052804414));
#10754=CARTESIAN_POINT('Ctrl Pts',(-0.953033902926841,2.261943850834,21.5929443870828));
#10755=CARTESIAN_POINT('Ctrl Pts',(-1.70054244388073,1.94699306978433,21.6352834937241));
#10756=CARTESIAN_POINT('Ctrl Pts',(-2.27648469868961,1.22484449224763,21.6776226003654));
#10757=CARTESIAN_POINT('Ctrl Pts',(-2.41726759477328,0.426005841826502,
21.7199617070068));
#10758=CARTESIAN_POINT('Ctrl Pts',(-2.44188549961531,0.286317467547558,
21.7273653059338));
#10759=CARTESIAN_POINT('Ctrl Pts',(-2.4531973065269,0.144284100337561,21.7347689048609));
#10760=CARTESIAN_POINT('Ctrl Pts',(-2.45192339561065,0.00204828064707867,
21.7421725037879));
#10761=CARTESIAN_POINT('Origin',(0.,0.,0.));
#10762=CARTESIAN_POINT('',(-2.44651884106482,-0.000297702156279583,22.6578274962121));
#10763=CARTESIAN_POINT('',(-2.44652741818257,0.000358158153537213,22.542172503788));
#10764=CARTESIAN_POINT('',(-2.4505,-3.00099698131059E-16,0.));
#10765=CARTESIAN_POINT('Ctrl Pts',(-2.44651884106482,-0.000297702156279583,
22.6578274962121));
#10766=CARTESIAN_POINT('Ctrl Pts',(-2.44605503950896,0.426777531908182,
22.6357216376468));
#10767=CARTESIAN_POINT('Ctrl Pts',(-2.3397784981325,0.854068794585224,22.6136157790816));
#10768=CARTESIAN_POINT('Ctrl Pts',(-2.12902721506848,1.22142322150288,22.5915099205163));
#10769=CARTESIAN_POINT('Ctrl Pts',(-1.72552733123021,1.9247521238646,22.5491865180984));
#10770=CARTESIAN_POINT('Ctrl Pts',(-0.939063686508212,2.40837590260392,
22.5068631156804));
#10771=CARTESIAN_POINT('Ctrl Pts',(-0.129335964024876,2.45110253453492,
22.4645397132624));
#10772=CARTESIAN_POINT('Ctrl Pts',(0.680391758458507,2.49382916646593,22.4222163108445));
#10773=CARTESIAN_POINT('Ctrl Pts',(1.51338355870323,2.09565865158857,22.3798929084265));
#10774=CARTESIAN_POINT('Ctrl Pts',(1.98866133778568,1.4386995033837,22.3375695060085));
#10775=CARTESIAN_POINT('Ctrl Pts',(2.46393911686811,0.781740355178845,22.2952461035906));
#10776=CARTESIAN_POINT('Ctrl Pts',(2.58150287478829,-0.134007426353506,
22.2529227011726));
#10777=CARTESIAN_POINT('Ctrl Pts',(2.28758310389872,-0.88971594965377,22.2105992987547));
#10778=CARTESIAN_POINT('Ctrl Pts',(1.99366333300913,-1.64542447295406,22.1682758963367));
#10779=CARTESIAN_POINT('Ctrl Pts',(1.28826003330977,-2.24109373802225,22.1259524939187));
#10780=CARTESIAN_POINT('Ctrl Pts',(0.493997970425276,-2.40428718126016,
22.0836290915008));
#10781=CARTESIAN_POINT('Ctrl Pts',(-0.300264092459193,-2.56748062449807,
22.0413056890828));
#10782=CARTESIAN_POINT('Ctrl Pts',(-1.18338491852879,-2.29819824590572,
21.9989822866649));
#10783=CARTESIAN_POINT('Ctrl Pts',(-1.75145877514209,-1.71959961745333,
21.9566588842469));
#10784=CARTESIAN_POINT('Ctrl Pts',(-2.19363752691133,-1.2692285674111,21.9237150882353));
#10785=CARTESIAN_POINT('Ctrl Pts',(-2.44493583356812,-0.631449196775602,
21.8907712922237));
#10786=CARTESIAN_POINT('Ctrl Pts',(-2.45077715073522,0.00222010580503924,
21.857827496212));
#10787=CARTESIAN_POINT('Ctrl Pts',(-2.45192339561065,0.00204828064707867,
21.7421725037879));
#10788=CARTESIAN_POINT('Ctrl Pts',(-2.44591216714184,-0.669122676207722,
21.7771080115022));
#10789=CARTESIAN_POINT('Ctrl Pts',(-2.15966337969236,-1.3448015037868,21.8120435192165));
#10790=CARTESIAN_POINT('Ctrl Pts',(-1.66886628902848,-1.7998746938669,21.8469790269308));
#10791=CARTESIAN_POINT('Ctrl Pts',(-1.07405854984159,-2.35138785583363,
21.8893181335722));
#10792=CARTESIAN_POINT('Ctrl Pts',(-0.178819534109371,-2.57888545646158,
21.9316572402135));
#10793=CARTESIAN_POINT('Ctrl Pts',(0.607124255160193,-2.37824804157426,
21.9739963468548));
#10794=CARTESIAN_POINT('Ctrl Pts',(1.39306804442971,-2.17761062668694,22.0163354534961));
#10795=CARTESIAN_POINT('Ctrl Pts',(2.06971660723662,-1.54883819628441,22.0586745601375));
#10796=CARTESIAN_POINT('Ctrl Pts',(2.32738634465144,-0.779702760243623,
22.1010136667788));
#10797=CARTESIAN_POINT('Ctrl Pts',(2.58505608206628,-0.0105673242027703,
22.1433527734202));
#10798=CARTESIAN_POINT('Ctrl Pts',(2.42374699408901,0.898931117476322,22.1856918800615));
#10799=CARTESIAN_POINT('Ctrl Pts',(1.9172858401876,1.53253992387863,22.2280309867028));
#10800=CARTESIAN_POINT('Ctrl Pts',(1.41082468628624,2.16614873028088,22.2703700933442));
#10801=CARTESIAN_POINT('Ctrl Pts',(0.559211466460781,2.52386790140634,22.3127091999855));
#10802=CARTESIAN_POINT('Ctrl Pts',(-0.247793631510701,2.44197910473602,
22.3550483066269));
#10803=CARTESIAN_POINT('Ctrl Pts',(-1.05479872948225,2.36009030806569,22.3973874132682));
#10804=CARTESIAN_POINT('Ctrl Pts',(-1.81719570559985,1.83859354359949,22.4397265199095));
#10805=CARTESIAN_POINT('Ctrl Pts',(-2.18605629215363,1.11616370017628,22.4820656265509));
#10806=CARTESIAN_POINT('Ctrl Pts',(-2.36060774707999,0.774296922188712,
22.5021012522966));
#10807=CARTESIAN_POINT('Ctrl Pts',(-2.44703253643979,0.387434147083485,
22.5221368780423));
#10808=CARTESIAN_POINT('Ctrl Pts',(-2.44652741818257,0.000358158153537213,
22.542172503788));
#10809=CARTESIAN_POINT('Origin',(0.,0.,0.));
#10810=CARTESIAN_POINT('',(-2.45183158050284,-0.00202607996204418,23.457827496212));
#10811=CARTESIAN_POINT('',(-2.45061074833635,-0.00223305219117096,23.342172503788));
#10812=CARTESIAN_POINT('',(-2.4505,-3.00099698131059E-16,0.));
#10813=CARTESIAN_POINT('Ctrl Pts',(-2.45183158050284,-0.00202607996204418,
23.457827496212));
#10814=CARTESIAN_POINT('Ctrl Pts',(-2.44582498250596,0.667196655845209,
23.4229953854879));
#10815=CARTESIAN_POINT('Ctrl Pts',(-2.16148734348512,1.34087475809766,23.3881632747638));
#10816=CARTESIAN_POINT('Ctrl Pts',(-1.67325809935663,1.79578569322896,23.3533311640396));
#10817=CARTESIAN_POINT('Ctrl Pts',(-1.08002609756608,2.3485336654773,23.3110077616217));
#10818=CARTESIAN_POINT('Ctrl Pts',(-0.185770244427078,2.57829563170229,
23.2686843592037));
#10819=CARTESIAN_POINT('Ctrl Pts',(0.600454879552817,2.37994277235467,23.2263609567858));
#10820=CARTESIAN_POINT('Ctrl Pts',(1.38668000353264,2.18158991300707,23.1840375543678));
#10821=CARTESIAN_POINT('Ctrl Pts',(2.06487439835336,1.55512222808694,23.1417141519498));
#10822=CARTESIAN_POINT('Ctrl Pts',(2.32488719844169,0.787085508260366,23.0993907495319));
#10823=CARTESIAN_POINT('Ctrl Pts',(2.58489999853004,0.0190487884337467,
23.0570673471139));
#10824=CARTESIAN_POINT('Ctrl Pts',(2.42673120388593,-0.890556966299377,
23.0147439446959));
#10825=CARTESIAN_POINT('Ctrl Pts',(1.92270575183184,-1.52572499032332,22.972420542278));
#10826=CARTESIAN_POINT('Ctrl Pts',(1.41868029977777,-2.16089301434725,22.93009713986));
#10827=CARTESIAN_POINT('Ctrl Pts',(0.568798190313761,-2.52162330766206,
22.8877737374421));
#10828=CARTESIAN_POINT('Ctrl Pts',(-0.238228768695827,-2.44292514296122,
22.8454503350241));
#10829=CARTESIAN_POINT('Ctrl Pts',(-1.04525572770542,-2.36422697826037,
22.8031269326061));
#10830=CARTESIAN_POINT('Ctrl Pts',(-1.80942753626056,-1.84610035554386,
22.7608035301882));
#10831=CARTESIAN_POINT('Ctrl Pts',(-2.18124537906091,-1.12552003119352,
22.7184801277702));
#10832=CARTESIAN_POINT('Ctrl Pts',(-2.35885972744917,-0.781304692287325,
22.6982625839175));
#10833=CARTESIAN_POINT('Ctrl Pts',(-2.44694302401464,-0.390891546210193,
22.6780450400648));
#10834=CARTESIAN_POINT('Ctrl Pts',(-2.44651884106482,-0.000297702156279583,
22.6578274962121));
#10835=CARTESIAN_POINT('Ctrl Pts',(-2.44652741818257,0.000358158153537213,
22.542172503788));
#10836=CARTESIAN_POINT('Ctrl Pts',(-2.44596512501825,-0.430531399968592,
22.5644759846836));
#10837=CARTESIAN_POINT('Ctrl Pts',(-2.33767976884795,-0.861685171488669,
22.5867794655792));
#10838=CARTESIAN_POINT('Ctrl Pts',(-2.12332222977882,-1.23132708371886,
22.6090829464749));
#10839=CARTESIAN_POINT('Ctrl Pts',(-1.71640338386024,-1.93302510181068,
22.6514220531162));
#10840=CARTESIAN_POINT('Ctrl Pts',(-0.927241495033076,-2.41305821561412,
22.6937611597576));
#10841=CARTESIAN_POINT('Ctrl Pts',(-0.117014635085855,-2.45172823427093,
22.7361002663989));
#10842=CARTESIAN_POINT('Ctrl Pts',(0.693212224861342,-2.49039825292774,
22.7784393730402));
#10843=CARTESIAN_POINT('Ctrl Pts',(1.5245040559286,-2.08770517643796,22.8207784796816));
#10844=CARTESIAN_POINT('Ctrl Pts',(1.99640159042075,-1.42795087439993,22.8631175863229));
#10845=CARTESIAN_POINT('Ctrl Pts',(2.4682991249129,-0.768196572361893,22.9054566929643));
#10846=CARTESIAN_POINT('Ctrl Pts',(2.58080236282996,0.148618955224388,22.9477957996056));
#10847=CARTESIAN_POINT('Ctrl Pts',(2.28242097573776,0.902894652953447,22.9901349062469));
#10848=CARTESIAN_POINT('Ctrl Pts',(1.98403958864555,1.65717035068253,23.0324740128883));
#10849=CARTESIAN_POINT('Ctrl Pts',(1.27477357654405,2.24890621855437,23.0748131195296));
#10850=CARTESIAN_POINT('Ctrl Pts',(0.479235925177236,2.40728006675578,23.117152226171));
#10851=CARTESIAN_POINT('Ctrl Pts',(-0.316301726189573,2.56565391495718,
23.1594913328123));
#10852=CARTESIAN_POINT('Ctrl Pts',(-1.19811101682169,2.29066574348813,23.2018304394536));
#10853=CARTESIAN_POINT('Ctrl Pts',(-1.76261427027663,1.70817168668717,23.244169546095));
#10854=CARTESIAN_POINT('Ctrl Pts',(-2.1981689528899,1.25873581101898,23.2768371986593));
#10855=CARTESIAN_POINT('Ctrl Pts',(-2.44482413436855,0.626234687516515,
23.3095048512236));
#10856=CARTESIAN_POINT('Ctrl Pts',(-2.45061074833635,-0.00223305219117096,
23.342172503788));
#10857=CARTESIAN_POINT('Origin',(0.,0.,-1.47904511860479));
#10858=CARTESIAN_POINT('',(-1.99583392989514,-0.00164926464131698,23.7209548813952));
#10859=CARTESIAN_POINT('',(-1.99764284170635,0.000851992992676968,23.8790451186048));
#10860=CARTESIAN_POINT('',(-1.99475,4.03981020633857E-13,-1.47904511860479));
#10861=CARTESIAN_POINT('',(-1.97959496748083,0.245420714742238,24.50525));
#10862=CARTESIAN_POINT('Ctrl Pts',(-1.99583392989514,-0.00164926464131691,
23.7209548813952));
#10863=CARTESIAN_POINT('Ctrl Pts',(-1.9968855024659,-0.118809805942343,
23.728446173089));
#10864=CARTESIAN_POINT('Ctrl Pts',(-1.93419140724538,-0.896774432952024,
23.7782608672008));
#10865=CARTESIAN_POINT('Ctrl Pts',(-0.911828861708041,-2.17415297545205,
23.8703989637307));
#10866=CARTESIAN_POINT('Ctrl Pts',(1.33175293478252,-1.94516872322012,23.9973691709844));
#10867=CARTESIAN_POINT('Ctrl Pts',(2.35590509889789,0.0621220732712832,
24.1243393782384));
#10868=CARTESIAN_POINT('Ctrl Pts',(1.22745053520999,2.01448000455152,24.2513095854922));
#10869=CARTESIAN_POINT('Ctrl Pts',(-1.02858118383587,2.12041610541359,24.3782797927461));
#10870=CARTESIAN_POINT('Ctrl Pts',(-1.89801534866759,0.903452385056865,
24.4629265975821));
#10871=CARTESIAN_POINT('Ctrl Pts',(-1.97959496748082,0.245420714742313,
24.50525));
#10872=CARTESIAN_POINT('',(-0.407652562758078,1.95265126189414,24.50525));
#10873=CARTESIAN_POINT('Origin',(0.,0.,24.50525));
#10874=CARTESIAN_POINT('Ctrl Pts',(-1.99764284170635,0.00085199299267695,
23.8790451186048));
#10875=CARTESIAN_POINT('Ctrl Pts',(-1.99436715728184,-0.613649439337014,
23.9184236525045));
#10876=CARTESIAN_POINT('Ctrl Pts',(-1.36122111898238,-1.89471011498649,
24.0001412930456));
#10877=CARTESIAN_POINT('Ctrl Pts',(0.817973374160278,-2.21053272043233,
24.1241980402279));
#10878=CARTESIAN_POINT('Ctrl Pts',(2.30301402245599,-0.512148340557086,
24.2512153601519));
#10879=CARTESIAN_POINT('Ctrl Pts',(1.674912756705,1.65836796725257,24.378232680076));
#10880=CARTESIAN_POINT('Ctrl Pts',(0.24166366648125,2.0882081993032,24.4629108933587));
#10881=CARTESIAN_POINT('Ctrl Pts',(-0.4076525627588,1.95265126189399,24.50525));
#10882=CARTESIAN_POINT('Origin',(0.,0.,-1.47904511860479));
#10883=CARTESIAN_POINT('',(-1.99150926676762,-0.00024233477887608,22.9209548813952));
#10884=CARTESIAN_POINT('',(-1.99484015108914,-0.0018177436674327,23.0790451186047));
#10885=CARTESIAN_POINT('',(-1.99475,4.03981020633857E-13,-1.47904511860479));
#10886=CARTESIAN_POINT('Ctrl Pts',(-1.99150926676762,-0.000242334778875961,
22.9209548813952));
#10887=CARTESIAN_POINT('Ctrl Pts',(-1.99185455913213,-0.318192577760585,
22.9411724252479));
#10888=CARTESIAN_POINT('Ctrl Pts',(-1.77005361978223,-1.30128478605611,
23.0037133715186));
#10889=CARTESIAN_POINT('Ctrl Pts',(-0.228807242491405,-2.34628640912002,
23.1085777202073));
#10890=CARTESIAN_POINT('Ctrl Pts',(1.84664960858395,-1.46536404316653,23.2355479274611));
#10891=CARTESIAN_POINT('Ctrl Pts',(2.23290613147693,0.755941093646845,23.3625181347151));
#10892=CARTESIAN_POINT('Ctrl Pts',(0.576719717599789,2.28580815893301,23.4894883419689));
#10893=CARTESIAN_POINT('Ctrl Pts',(-1.47825392840529,1.75782191898924,23.608967257529));
#10894=CARTESIAN_POINT('Ctrl Pts',(-1.99094445372519,0.543109785451063,
23.686122770671));
#10895=CARTESIAN_POINT('Ctrl Pts',(-1.99583392989514,-0.00164926464131691,
23.7209548813952));
#10896=CARTESIAN_POINT('Ctrl Pts',(-1.99484015108914,-0.00181774366743258,
23.0790451186047));
#10897=CARTESIAN_POINT('Ctrl Pts',(-1.9962346947758,-0.153275180353312,
23.0887165726818));
#10898=CARTESIAN_POINT('Ctrl Pts',(-1.91131516926029,-0.9662262501804,23.1407271334001));
#10899=CARTESIAN_POINT('Ctrl Pts',(-0.798085058971124,-2.21852563316919,
23.2350768007599));
#10900=CARTESIAN_POINT('Ctrl Pts',(1.43108576045911,-1.87368610656973,23.3620941206838));
#10901=CARTESIAN_POINT('Ctrl Pts',(2.35037186943588,0.186189415184726,23.4891114406079));
#10902=CARTESIAN_POINT('Ctrl Pts',(1.11815436836127,2.07570231768813,23.6161287605319));
#10903=CARTESIAN_POINT('Ctrl Pts',(-1.13736772283233,2.06510660675428,23.7431460804559));
#10904=CARTESIAN_POINT('Ctrl Pts',(-1.97555308243499,0.753708357097197,
23.8307848664802));
#10905=CARTESIAN_POINT('Ctrl Pts',(-1.99788911552757,0.0470516863299492,
23.8760845458631));
#10906=CARTESIAN_POINT('Ctrl Pts',(-1.99764284170635,0.00085199299267695,
23.8790451186048));
#10907=CARTESIAN_POINT('Origin',(0.,0.,-1.47904511860479));
#10908=CARTESIAN_POINT('',(-1.99497560556175,0.00180720508266196,22.1209548813952));
#10909=CARTESIAN_POINT('',(-1.99151624869198,0.000291547022211042,22.2790451186048));
#10910=CARTESIAN_POINT('',(-1.99475,4.03981020633857E-13,-1.47904511860479));
#10911=CARTESIAN_POINT('Ctrl Pts',(-1.99497560556175,0.00180720508266202,
22.1209548813952));
#10912=CARTESIAN_POINT('Ctrl Pts',(-1.99022067088762,-0.514010726491639,
22.1538986774068));
#10913=CARTESIAN_POINT('Ctrl Pts',(-1.52285647342705,-1.7001518019312,22.2291658758364));
#10914=CARTESIAN_POINT('Ctrl Pts',(0.474455608801953,-2.30917486244222,
22.3467564766839));
#10915=CARTESIAN_POINT('Ctrl Pts',(2.19708760073256,-0.854519159734979,
22.4737266839378));
#10916=CARTESIAN_POINT('Ctrl Pts',(1.90999071506285,1.3817851298529,22.6006968911917));
#10917=CARTESIAN_POINT('Ctrl Pts',(-0.124219111753841,2.35413848780229,
22.7276670984456));
#10918=CARTESIAN_POINT('Ctrl Pts',(-1.73898870880108,1.36116064380626,22.8344197618468));
#10919=CARTESIAN_POINT('Ctrl Pts',(-1.99113172416258,0.347404399826265,
22.89884902283));
#10920=CARTESIAN_POINT('Ctrl Pts',(-1.99150926676762,-0.000242334778875961,
22.9209548813952));
#10921=CARTESIAN_POINT('Ctrl Pts',(-1.99151624869198,0.000291547022210972,
22.2790451186048));
#10922=CARTESIAN_POINT('Ctrl Pts',(-1.99105853218949,-0.3504601142977,22.3013485995004));
#10923=CARTESIAN_POINT('Ctrl Pts',(-1.73558284268583,-1.36767343802751,
22.3659911870374));
#10924=CARTESIAN_POINT('Ctrl Pts',(-0.112399222395231,-2.35502710849036,
22.4729728812157));
#10925=CARTESIAN_POINT('Ctrl Pts',(1.91765919019992,-1.37162941700542,22.5999902011398));
#10926=CARTESIAN_POINT('Ctrl Pts',(2.19239801962464,0.867282364654784,22.7270075210638));
#10927=CARTESIAN_POINT('Ctrl Pts',(0.460333080665931,2.31233250434551,22.8540248409878));
#10928=CARTESIAN_POINT('Ctrl Pts',(-1.52912384593445,1.69192951214063,22.9713707068348));
#10929=CARTESIAN_POINT('Ctrl Pts',(-1.99012974577896,0.509766024453988,
23.0463774660404));
#10930=CARTESIAN_POINT('Ctrl Pts',(-1.99484015108914,-0.00181774366743258,
23.0790451186047));
#10931=CARTESIAN_POINT('Origin',(0.,0.,-1.47904511860479));
#10932=CARTESIAN_POINT('',(-1.99749018587619,-0.000921389143520827,21.3209548813952));
#10933=CARTESIAN_POINT('',(-1.99590866900402,0.00166733638921758,21.4790451186048));
#10934=CARTESIAN_POINT('',(-1.99475,4.03981020633857E-13,-1.47904511860479));
#10935=CARTESIAN_POINT('Ctrl Pts',(-1.99749018587619,-0.000921389143520883,
21.3209548813952));
#10936=CARTESIAN_POINT('Ctrl Pts',(-1.99778999557661,-0.0531502469707051,
21.3243015271478));
#10937=CARTESIAN_POINT('Ctrl Pts',(-1.97225597155269,-0.765594304990007,
21.3699715753183));
#10938=CARTESIAN_POINT('Ctrl Pts',(-1.1192673629799,-2.07476191756569,21.4579650259067));
#10939=CARTESIAN_POINT('Ctrl Pts',(1.13537360904899,-2.06599206652615,21.5849352331606));
#10940=CARTESIAN_POINT('Ctrl Pts',(2.3514613175128,-0.167410083297791,21.7119054404145));
#10941=CARTESIAN_POINT('Ctrl Pts',(1.41661136721561,1.88430587953843,21.8388756476684));
#10942=CARTESIAN_POINT('Ctrl Pts',(-0.814046703622753,2.21240241272419,
21.9658458549223));
#10943=CARTESIAN_POINT('Ctrl Pts',(-1.91451027631426,0.956714097230605,
22.0598722661646));
#10944=CARTESIAN_POINT('Ctrl Pts',(-1.99632940873961,0.14866851923707,22.1115752749889));
#10945=CARTESIAN_POINT('Ctrl Pts',(-1.99497560556175,0.00180720508266202,
22.1209548813952));
#10946=CARTESIAN_POINT('Ctrl Pts',(-1.99590866900402,0.00166733638921734,
21.4790451186048));
#10947=CARTESIAN_POINT('Ctrl Pts',(-1.99101542354886,-0.54467759982231,
21.5139806263191));
#10948=CARTESIAN_POINT('Ctrl Pts',(-1.47561210593682,-1.76126654148221,
21.5912552406747));
#10949=CARTESIAN_POINT('Ctrl Pts',(0.583178029368184,-2.28444505330724,
21.7108689616716));
#10950=CARTESIAN_POINT('Ctrl Pts',(2.23558944009154,-0.748949678226114,
21.8378862815957));
#10951=CARTESIAN_POINT('Ctrl Pts',(1.84166415556682,1.47209339446037,21.9649036015196));
#10952=CARTESIAN_POINT('Ctrl Pts',(-0.23802015814085,2.34566244151516,22.0919209214437));
#10953=CARTESIAN_POINT('Ctrl Pts',(-1.77291039590186,1.29576282507227,22.196634760472));
#10954=CARTESIAN_POINT('Ctrl Pts',(-1.99192742381681,0.315378194203477,
22.2590094928591));
#10955=CARTESIAN_POINT('Ctrl Pts',(-1.99151624869198,0.000291547022210972,
22.2790451186048));
#10956=CARTESIAN_POINT('Origin',(0.,0.,-1.47904511860479));
#10957=CARTESIAN_POINT('',(-1.99224100758391,-0.00120392385877232,20.5209548813952));
#10958=CARTESIAN_POINT('',(-1.99684525596436,-0.00133650482941783,20.6790451186048));
#10959=CARTESIAN_POINT('',(-1.99475,4.03981020633857E-13,-1.47904511860479));
#10960=CARTESIAN_POINT('Ctrl Pts',(-1.99224100758391,-0.00120392385877197,
20.5209548813952));
#10961=CARTESIAN_POINT('Ctrl Pts',(-1.99363325941504,-0.253741713763136,
20.5370277793067));
#10962=CARTESIAN_POINT('Ctrl Pts',(-1.83189848440572,-1.16954880445064,
20.5954240796361));
#10963=CARTESIAN_POINT('Ctrl Pts',(-0.456477659862079,-2.31279583952387,
20.6961437823834));
#10964=CARTESIAN_POINT('Ctrl Pts',(1.6949690987159,-1.63843712229916,20.8231139896373));
#10965=CARTESIAN_POINT('Ctrl Pts',(2.29598727142038,0.534639036362976,20.9500841968912));
#10966=CARTESIAN_POINT('Ctrl Pts',(0.796811227132131,2.21866814035183,21.0770544041451));
#10967=CARTESIAN_POINT('Ctrl Pts',(-1.3725009971516,1.88233367605118,21.2006779656464));
#10968=CARTESIAN_POINT('Ctrl Pts',(-1.99399844799794,0.607362735608021,
21.2819781247298));
#10969=CARTESIAN_POINT('Ctrl Pts',(-1.99749018587619,-0.000921389143520883,
21.3209548813952));
#10970=CARTESIAN_POINT('Ctrl Pts',(-1.99684525596436,-0.00133650482941808,
20.6790451186048));
#10971=CARTESIAN_POINT('Ctrl Pts',(-1.99747501960825,-0.0830024421592919,
20.6842735464963));
#10972=CARTESIAN_POINT('Ctrl Pts',(-1.95584301886423,-0.825340921944485,
20.7318410810293));
#10973=CARTESIAN_POINT('Ctrl Pts',(-1.02554856753737,-2.12297808204117,
20.8217477222035));
#10974=CARTESIAN_POINT('Ctrl Pts',(1.22747389894261,-2.0129812788532,20.9487650421275));
#10975=CARTESIAN_POINT('Ctrl Pts',(2.35693366377738,-0.0604111340540538,
21.0757823620516));
#10976=CARTESIAN_POINT('Ctrl Pts',(1.32898482224672,1.94745606972551,21.2027996819756));
#10977=CARTESIAN_POINT('Ctrl Pts',(-0.915444287757947,2.1727281375204,21.3298170018996));
#10978=CARTESIAN_POINT('Ctrl Pts',(-1.93507962172209,0.894252387772451,
21.4218988141093));
#10979=CARTESIAN_POINT('Ctrl Pts',(-1.9969456548437,0.117449789491568,21.4716415196777));
#10980=CARTESIAN_POINT('Ctrl Pts',(-1.99590866900402,0.00166733638921734,
21.4790451186048));
#10981=CARTESIAN_POINT('Origin',(0.,0.,-1.47904511860479));
#10982=CARTESIAN_POINT('',(-1.99312087176262,0.00161274543637441,19.7209548813952));
#10983=CARTESIAN_POINT('',(-1.99180439006996,-0.000824340204725049,19.8790451186048));
#10984=CARTESIAN_POINT('',(-1.99475,4.03981020633857E-13,-1.47904511860479));
#10985=CARTESIAN_POINT('Ctrl Pts',(-1.99312087176262,0.00161274543637444,
19.7209548813952));
#10986=CARTESIAN_POINT('Ctrl Pts',(-1.98968192268936,-0.450377960742678,
19.7497540314656));
#10987=CARTESIAN_POINT('Ctrl Pts',(-1.61339717903016,-1.57179914144911,
19.8208765839539));
#10988=CARTESIAN_POINT('Ctrl Pts',(0.247048790610012,-2.34443241412816,
19.9343225388601));
#10989=CARTESIAN_POINT('Ctrl Pts',(2.10330301895634,-1.0646656093841,20.061292746114));
#10990=CARTESIAN_POINT('Ctrl Pts',(2.0356159034317,1.18897617430391,20.1882629533679));
#10991=CARTESIAN_POINT('Ctrl Pts',(0.10590245999703,2.35503314590555,20.3152331606218));
#10992=CARTESIAN_POINT('Ctrl Pts',(-1.66414125646537,1.49197284957946,20.4261304699642));
#10993=CARTESIAN_POINT('Ctrl Pts',(-1.98996716044266,0.411244685500659,
20.4947043768887));
#10994=CARTESIAN_POINT('Ctrl Pts',(-1.99224100758391,-0.00120392385877197,
20.5209548813952));
#10995=CARTESIAN_POINT('Ctrl Pts',(-1.99180439006996,-0.000824340204724841,
19.8790451186048));
#10996=CARTESIAN_POINT('Ctrl Pts',(-1.99284937662136,-0.281602094708555,
19.896905573315));
#10997=CARTESIAN_POINT('Ctrl Pts',(-1.80623847218132,-1.22665110166896,
19.9571051346665));
#10998=CARTESIAN_POINT('Ctrl Pts',(-0.357873132381371,-2.33038894229026,
20.0596438026594));
#10999=CARTESIAN_POINT('Ctrl Pts',(1.76383231338145,-1.56450675022861,20.1866611225834));
#11000=CARTESIAN_POINT('Ctrl Pts',(2.27102180036648,0.633439644702114,20.3136784425075));
#11001=CARTESIAN_POINT('Ctrl Pts',(0.699441717491183,2.25156991564901,20.4406957624314));
#11002=CARTESIAN_POINT('Ctrl Pts',(-1.42132417394977,1.82696424060745,20.5624846544639));
#11003=CARTESIAN_POINT('Ctrl Pts',(-1.99237527822705,0.578317346747391,
20.641934439855));
#11004=CARTESIAN_POINT('Ctrl Pts',(-1.99684525596436,-0.00133650482941808,
20.6790451186048));
#11005=CARTESIAN_POINT('Origin',(0.,0.,-1.47904511860479));
#11006=CARTESIAN_POINT('',(-1.99798271913518,0.000231452487769965,18.9209548813952));
#11007=CARTESIAN_POINT('',(-1.99382977638889,0.0017725417048866,19.0790451186048));
#11008=CARTESIAN_POINT('',(-1.99475,4.03981020633857E-13,-1.47904511860479));
#11009=CARTESIAN_POINT('Ctrl Pts',(-1.99798271913518,0.000231452487770123,
18.9209548813952));
#11010=CARTESIAN_POINT('Ctrl Pts',(-1.99691903787442,-0.647402032613039,
18.9624802836245));
#11011=CARTESIAN_POINT('Ctrl Pts',(-1.30211730807037,-1.95707393283707,
19.0463290882716));
#11012=CARTESIAN_POINT('Ctrl Pts',(0.928528238935361,-2.16684834699098,
19.1725012953368));
#11013=CARTESIAN_POINT('Ctrl Pts',(2.32393504393153,-0.395881751214744,
19.2994715025907));
#11014=CARTESIAN_POINT('Ctrl Pts',(1.59358313931722,1.73720730698498,19.4264417098446));
#11015=CARTESIAN_POINT('Ctrl Pts',(-0.594457200581991,2.28123148453506,
19.5534119170984));
#11016=CARTESIAN_POINT('Ctrl Pts',(-1.86578167130184,1.08846508423875,19.651582974282));
#11017=CARTESIAN_POINT('Ctrl Pts',(-1.99473582272346,0.213870272280659,
19.7074306290476));
#11018=CARTESIAN_POINT('Ctrl Pts',(-1.99312087176262,0.00161274543637444,
19.7209548813952));
#11019=CARTESIAN_POINT('Ctrl Pts',(-1.99382977638889,0.00177254170488682,
19.0790451186048));
#11020=CARTESIAN_POINT('Ctrl Pts',(-1.98972515875545,-0.476363613015602,
19.1095376001336));
#11021=CARTESIAN_POINT('Ctrl Pts',(-1.57755368547404,-1.62474792733362,
19.1823691883038));
#11022=CARTESIAN_POINT('Ctrl Pts',(0.341271742863524,-2.33287792195687,
19.2975398831153));
#11023=CARTESIAN_POINT('Ctrl Pts',(2.14508879272012,-0.978457905368288,
19.4245572030393));
#11024=CARTESIAN_POINT('Ctrl Pts',(1.98540848369728,1.27158914516195,19.5515745229634));
#11025=CARTESIAN_POINT('Ctrl Pts',(0.00839346700838828,2.35769280249617,
19.6785918428874));
#11026=CARTESIAN_POINT('Ctrl Pts',(-1.69722751078314,1.43643151043362,19.7877487081012));
#11027=CARTESIAN_POINT('Ctrl Pts',(-1.9903721834168,0.383995701278938,19.8545664666736));
#11028=CARTESIAN_POINT('Ctrl Pts',(-1.99180439006996,-0.000824340204724841,
19.8790451186048));
#11029=CARTESIAN_POINT('Origin',(0.,0.,-1.47904511860479));
#11030=CARTESIAN_POINT('',(-1.99379303657575,-0.00176355010682069,18.1209548813952));
#11031=CARTESIAN_POINT('',(-1.99798916403529,-0.000228181391768167,18.2790451186048));
#11032=CARTESIAN_POINT('',(-1.99475,4.03981020633857E-13,-1.47904511860479));
#11033=CARTESIAN_POINT('Ctrl Pts',(-1.99379303657575,-0.00176355010682052,
18.1209548813952));
#11034=CARTESIAN_POINT('Ctrl Pts',(-1.99538935452561,-0.188812871833617,
18.1328831333654));
#11035=CARTESIAN_POINT('Ctrl Pts',(-1.88545983445616,-1.03770416276352,
18.1871347877535));
#11036=CARTESIAN_POINT('Ctrl Pts',(-0.679802134300005,-2.25726948049166,
18.2837098445596));
#11037=CARTESIAN_POINT('Ctrl Pts',(1.52714444375655,-1.79589150486922,18.4106800518135));
#11038=CARTESIAN_POINT('Ctrl Pts',(2.33717564303521,0.30823118427704,18.5376502590674));
#11039=CARTESIAN_POINT('Ctrl Pts',(1.00933664148997,2.13040747123729,18.6646204663213));
#11040=CARTESIAN_POINT('Ctrl Pts',(-1.24176661487133,2.00384932655849,18.7915906735751));
#11041=CARTESIAN_POINT('Ctrl Pts',(-1.99226228190403,0.685182598197949,
18.8770354785998));
#11042=CARTESIAN_POINT('Ctrl Pts',(-1.99800316006534,0.0126771270771923,
18.9201568812065));
#11043=CARTESIAN_POINT('Ctrl Pts',(-1.99798271913518,0.000231452487770123,
18.9209548813952));
#11044=CARTESIAN_POINT('Ctrl Pts',(-1.99798916403529,-0.000228181391767968,
18.2790451186048));
#11045=CARTESIAN_POINT('Ctrl Pts',(-1.99800899793164,-0.012477266092771,
18.2798305203109));
#11046=CARTESIAN_POINT('Ctrl Pts',(-1.99235887395581,-0.685026095535388,
18.3229550286584));
#11047=CARTESIAN_POINT('Ctrl Pts',(-1.24177516838345,-2.00419066768041,
18.4084186436472));
#11048=CARTESIAN_POINT('Ctrl Pts',(1.01040701496368,-2.13022615356754,18.5354359635712));
#11049=CARTESIAN_POINT('Ctrl Pts',(2.33771769089012,-0.306368730340369,
18.6624532834953));
#11050=CARTESIAN_POINT('Ctrl Pts',(1.52520901414179,1.79792192945402,18.7894706034193));
#11051=CARTESIAN_POINT('Ctrl Pts',(-0.683392859853091,2.25649285403983,
18.9164879233433));
#11052=CARTESIAN_POINT('Ctrl Pts',(-1.8864156933587,1.03535444444075,19.0130127617384));
#11053=CARTESIAN_POINT('Ctrl Pts',(-1.99542446018947,0.187533079834375,
19.0671984934923));
#11054=CARTESIAN_POINT('Ctrl Pts',(-1.99382977638889,0.00177254170488682,
19.0790451186048));
#11055=CARTESIAN_POINT('Origin',(0.,0.,-1.47904511860479));
#11056=CARTESIAN_POINT('',(-1.99184618389856,0.000865127372006838,17.3209548813952));
#11057=CARTESIAN_POINT('',(-1.99316281920955,-0.00162934947814997,17.4790451186048));
#11058=CARTESIAN_POINT('',(-1.99475,4.03981020633857E-13,-1.47904511860479));
#11059=CARTESIAN_POINT('Ctrl Pts',(-1.99184618389856,0.000865127372006828,
17.3209548813952));
#11060=CARTESIAN_POINT('Ctrl Pts',(-1.99032959737337,-0.386699381348846,
17.3456093855243));
#11061=CARTESIAN_POINT('Ctrl Pts',(-1.69406802365858,-1.44172282084515,
17.4125872920713));
#11062=CARTESIAN_POINT('Ctrl Pts',(0.0172877380261932,-2.35734969477841,
17.5218886010363));
#11063=CARTESIAN_POINT('Ctrl Pts',(1.98947600304585,-1.26466662906185,17.6488588082902));
#11064=CARTESIAN_POINT('Ctrl Pts',(2.14184320547626,0.984837109634436,17.775829015544));
#11065=CARTESIAN_POINT('Ctrl Pts',(0.335015437913597,2.33348689855279,17.902799222798));
#11066=CARTESIAN_POINT('Ctrl Pts',(-1.57972676945643,1.62146721495462,18.0178411780816));
#11067=CARTESIAN_POINT('Ctrl Pts',(-1.98972535554673,0.474868926241488,
18.0905597309474));
#11068=CARTESIAN_POINT('Ctrl Pts',(-1.99379303657575,-0.00176355010682052,
18.1209548813952));
#11069=CARTESIAN_POINT('Ctrl Pts',(-1.99316281920955,-0.00162934947815016,
17.4790451186048));
#11070=CARTESIAN_POINT('Ctrl Pts',(-1.99478285074208,-0.212199013029784,
17.4924625471296));
#11071=CARTESIAN_POINT('Ctrl Pts',(-1.86711225706861,-1.08531368698141,
17.5482190822957));
#11072=CARTESIAN_POINT('Ctrl Pts',(-0.599428442729515,-2.28023493159759,
17.6463147241031));
#11073=CARTESIAN_POINT('Ctrl Pts',(1.5906925238854,-1.74025374462637,17.7733320440271));
#11074=CARTESIAN_POINT('Ctrl Pts',(2.32478025773261,0.392660864471763,17.9003493639512));
#11075=CARTESIAN_POINT('Ctrl Pts',(0.930890860039063,2.16615512092895,18.0273666838751));
#11076=CARTESIAN_POINT('Ctrl Pts',(-1.3011974724079,1.95816315404478,18.1535986020931));
#11077=CARTESIAN_POINT('Ctrl Pts',(-1.99693980054367,0.64784126818084,18.2374914136696));
#11078=CARTESIAN_POINT('Ctrl Pts',(-1.99798916403529,-0.000228181391767968,
18.2790451186048));
#11079=CARTESIAN_POINT('Origin',(0.,0.,-1.47904511860479));
#11080=CARTESIAN_POINT('',(-1.99695131403112,0.00127851392262751,16.5209548813952));
#11081=CARTESIAN_POINT('',(-1.99217715215978,0.00116458179186874,16.6790451186048));
#11082=CARTESIAN_POINT('',(-1.99475,4.03981020633857E-13,-1.47904511860479));
#11083=CARTESIAN_POINT('Ctrl Pts',(-1.99695131403112,0.0012785139226276,
16.5209548813952));
#11084=CARTESIAN_POINT('Ctrl Pts',(-1.99259585846887,-0.58251261776068,
16.5583356376832));
#11085=CARTESIAN_POINT('Ctrl Pts',(-1.41447577495437,-1.83479432529662,
16.6380397963891));
#11086=CARTESIAN_POINT('Ctrl Pts',(0.712834826853045,-2.24705650996661,
16.760067357513));
#11087=CARTESIAN_POINT('Ctrl Pts',(2.27426375960074,-0.620581018985151,
16.8870375647669));
#11088=CARTESIAN_POINT('Ctrl Pts',(1.75536948901827,1.57355470396859,17.0140077720207));
#11089=CARTESIAN_POINT('Ctrl Pts',(-0.36920304249889,2.32832247825929,17.1409779792746));
#11090=CARTESIAN_POINT('Ctrl Pts',(-1.80909353809998,1.2203103924296,17.2432936823995));
#11091=CARTESIAN_POINT('Ctrl Pts',(-1.99293306088134,0.278617129567366,
17.3032859831063));
#11092=CARTESIAN_POINT('Ctrl Pts',(-1.99184618389856,0.000865127372006828,
17.3209548813952));
#11093=CARTESIAN_POINT('Ctrl Pts',(-1.99217715215978,0.00116458179186867,
16.6790451186048));
#11094=CARTESIAN_POINT('Ctrl Pts',(-1.98999999646129,-0.40815773762222,
16.7050945739482));
#11095=CARTESIAN_POINT('Ctrl Pts',(-1.66793149151012,-1.48590988532565,
16.7734831359329));
#11096=CARTESIAN_POINT('Ctrl Pts',(0.0956287989740662,-2.355767589139,16.884210804559));
#11097=CARTESIAN_POINT('Ctrl Pts',(2.03110108030785,-1.19725277314494,17.011228124483));
#11098=CARTESIAN_POINT('Ctrl Pts',(2.10741414159636,1.05716197294014,17.138245444407));
#11099=CARTESIAN_POINT('Ctrl Pts',(0.254715166118652,2.34390827153712,17.2652627643311));
#11100=CARTESIAN_POINT('Ctrl Pts',(-1.61079803731833,1.57588134084248,17.3788626557303));
#11101=CARTESIAN_POINT('Ctrl Pts',(-1.98967079162499,0.45226000935907,17.4501234404882));
#11102=CARTESIAN_POINT('Ctrl Pts',(-1.99316281920955,-0.00162934947815016,
17.4790451186048));
#11103=CARTESIAN_POINT('Origin',(0.,0.,-1.47904511860479));
#11104=CARTESIAN_POINT('',(-1.99572977164192,-0.00170384222700574,15.7209548813952));
#11105=CARTESIAN_POINT('',(-1.99740160550243,0.000998204556411052,15.8790451186048));
#11106=CARTESIAN_POINT('',(-1.99475,4.03981020633857E-13,-1.47904511860479));
#11107=CARTESIAN_POINT('Ctrl Pts',(-1.99572977164192,-0.00170384222700588,
15.7209548813952));
#11108=CARTESIAN_POINT('Ctrl Pts',(-1.99683270343229,-0.123457329418355,
15.7287384874241));
#11109=CARTESIAN_POINT('Ctrl Pts',(-1.93126068112857,-0.906060978578068,
15.7788454958709));
#11110=CARTESIAN_POINT('Ctrl Pts',(-0.896648704865739,-2.18023337040339,
15.8712759067358));
#11111=CARTESIAN_POINT('Ctrl Pts',(1.34476747364227,-1.93623265420035,15.9982461139896));
#11112=CARTESIAN_POINT('Ctrl Pts',(2.35609282970634,0.0788861658613507,
16.1252163212435));
#11113=CARTESIAN_POINT('Ctrl Pts',(1.21224398394502,2.02184593200051,16.2521865284974));
#11114=CARTESIAN_POINT('Ctrl Pts',(-1.04047329330418,2.11537509091856,16.3791567357513));
#11115=CARTESIAN_POINT('Ctrl Pts',(-1.95843139238505,0.816055134121286,
16.4687461867172));
#11116=CARTESIAN_POINT('Ctrl Pts',(-1.99752721130333,0.0784699157103159,
16.5160122352652));
#11117=CARTESIAN_POINT('Ctrl Pts',(-1.99695131403112,0.0012785139226276,
16.5209548813952));
#11118=CARTESIAN_POINT('Ctrl Pts',(-1.99740160550243,0.00099820455641106,
15.8790451186048));
#11119=CARTESIAN_POINT('Ctrl Pts',(-1.99370023614505,-0.602748628883622,
15.9177266007668));
#11120=CARTESIAN_POINT('Ctrl Pts',(-1.38028516085263,-1.87384538130254,
15.9987471895702));
#11121=CARTESIAN_POINT('Ctrl Pts',(0.782276957985213,-2.22414670429727,
16.1221068850149));
#11122=CARTESIAN_POINT('Ctrl Pts',(2.2929055224434,-0.548971826580871,16.249124204939));
#11123=CARTESIAN_POINT('Ctrl Pts',(1.704733350654,1.62870193847707,16.3761415248629));
#11124=CARTESIAN_POINT('Ctrl Pts',(-0.443858810723858,2.31555072442255,
16.503158844787));
#11125=CARTESIAN_POINT('Ctrl Pts',(-1.82884408866752,1.17669301721355,16.6041267093676));
#11126=CARTESIAN_POINT('Ctrl Pts',(-1.99353860508394,0.257128392313624,
16.6627554673068));
#11127=CARTESIAN_POINT('Ctrl Pts',(-1.99217715215978,0.00116458179186867,
16.6790451186048));
#11128=CARTESIAN_POINT('Origin',(0.,0.,-1.47904511860479));
#11129=CARTESIAN_POINT('',(-1.99149560426942,-0.000167792983348677,14.9209548813952));
#11130=CARTESIAN_POINT('',(-1.99517067278375,-0.00179390005510177,15.0790451186048));
#11131=CARTESIAN_POINT('',(-1.99475,4.03981020633857E-13,-1.47904511860479));
#11132=CARTESIAN_POINT('Ctrl Pts',(-1.99149560426942,-0.000167792983348583,
14.9209548813952));
#11133=CARTESIAN_POINT('Ctrl Pts',(-1.99173785851776,-0.322720966835465,
14.941464739583));
#11134=CARTESIAN_POINT('Ctrl Pts',(-1.76536638897614,-1.31056254377754,
15.0042980001888));
#11135=CARTESIAN_POINT('Ctrl Pts',(-0.21263805117564,-2.34780354982058,
15.1094546632124));
#11136=CARTESIAN_POINT('Ctrl Pts',(1.85669106744545,-1.45261651148066,15.2364248704663));
#11137=CARTESIAN_POINT('Ctrl Pts',(2.22766066522509,0.771313431729834,15.3633950777202));
#11138=CARTESIAN_POINT('Ctrl Pts',(0.560936019559882,2.28970461660849,15.4903652849741));
#11139=CARTESIAN_POINT('Ctrl Pts',(-1.48526110718087,1.74896222764933,15.6095518861991));
#11140=CARTESIAN_POINT('Ctrl Pts',(-1.99083550549725,0.538577955392992,
15.6864150850061));
#11141=CARTESIAN_POINT('Ctrl Pts',(-1.99572977164192,-0.00170384222700588,
15.7209548813952));
#11142=CARTESIAN_POINT('Ctrl Pts',(-1.99517067278375,-0.00179390005510177,
15.0790451186048));
#11143=CARTESIAN_POINT('Ctrl Pts',(-1.99646803238674,-0.14227544571559,
15.0880195209441));
#11144=CARTESIAN_POINT('Ctrl Pts',(-1.91885345210777,-0.944092523599761,
15.1393330299248));
#11145=CARTESIAN_POINT('Ctrl Pts',(-0.834420476588558,-2.20511411711067,
15.2329856455468));
#11146=CARTESIAN_POINT('Ctrl Pts',(1.40013588510504,-1.89694631038207,15.3600029654708));
#11147=CARTESIAN_POINT('Ctrl Pts',(2.35308417453332,0.147582752352149,15.4870202853949));
#11148=CARTESIAN_POINT('Ctrl Pts',(1.15214746973809,2.05702260785027,15.6140376053188));
#11149=CARTESIAN_POINT('Ctrl Pts',(-1.10340222895637,2.08357608989091,15.7410549252429));
#11150=CARTESIAN_POINT('Ctrl Pts',(-1.9696398684246,0.775661723098001,15.8293907630048));
#11151=CARTESIAN_POINT('Ctrl Pts',(-1.99775159775743,0.0580869993455256,
15.8753874941255));
#11152=CARTESIAN_POINT('Ctrl Pts',(-1.99740160550243,0.00099820455641106,
15.8790451186048));
#11153=CARTESIAN_POINT('Origin',(0.,0.,-1.47904511860479));
#11154=CARTESIAN_POINT('',(-1.99511464393632,0.00179586406614344,14.1209548813952));
#11155=CARTESIAN_POINT('',(-1.99148314676551,0.000112721033546509,14.2790451186048));
#11156=CARTESIAN_POINT('',(-1.99475,4.03981020633857E-13,-1.47904511860479));
#11157=CARTESIAN_POINT('Ctrl Pts',(-1.99511464393632,0.00179586406614349,
14.1209548813952));
#11158=CARTESIAN_POINT('Ctrl Pts',(-1.99031466719488,-0.518505987664431,
14.1541909917419));
#11159=CARTESIAN_POINT('Ctrl Pts',(-1.51608605094631,-1.70912036928094,
14.2297505045065));
#11160=CARTESIAN_POINT('Ctrl Pts',(0.490348739021751,-2.30585224233855,
14.3476334196891));
#11161=CARTESIAN_POINT('Ctrl Pts',(2.20292078401032,-0.839366706948347,
14.474603626943));
#11162=CARTESIAN_POINT('Ctrl Pts',(1.90042874387294,1.39490753773124,14.6015738341969));
#11163=CARTESIAN_POINT('Ctrl Pts',(-0.140430710978244,2.35322664968167,
14.7285440414508));
#11164=CARTESIAN_POINT('Ctrl Pts',(-1.74391877908516,1.35190122394337,14.8350043905169));
#11165=CARTESIAN_POINT('Ctrl Pts',(-1.99123795140256,0.342888110182512,
14.899141337165));
#11166=CARTESIAN_POINT('Ctrl Pts',(-1.99149560426942,-0.000167792983348583,
14.9209548813952));
#11167=CARTESIAN_POINT('Ctrl Pts',(-1.99148314676551,0.000112721033546474,
14.2790451186048));
#11168=CARTESIAN_POINT('Ctrl Pts',(-1.99131185922732,-0.339690971417257,
14.3006515477628));
#11169=CARTESIAN_POINT('Ctrl Pts',(-1.74734127274221,-1.34559130575002,
14.3645970835621));
#11170=CARTESIAN_POINT('Ctrl Pts',(-0.151061206087832,-2.35286342851562,
14.4708817260027));
#11171=CARTESIAN_POINT('Ctrl Pts',(1.89487438652815,-1.40293865172736,14.5978990459267));
#11172=CARTESIAN_POINT('Ctrl Pts',(2.2063452493004,0.831159697122361,14.7249163658507));
#11173=CARTESIAN_POINT('Ctrl Pts',(0.498247931734623,2.30445976310136,14.8519336857748));
#11174=CARTESIAN_POINT('Ctrl Pts',(-1.51300932258991,1.7133249444358,14.9699766033595));
#11175=CARTESIAN_POINT('Ctrl Pts',(-1.99034739677153,0.520483244831458,
15.0456804143028));
#11176=CARTESIAN_POINT('Ctrl Pts',(-1.99517067278375,-0.00179390005510177,
15.0790451186048));
#11177=CARTESIAN_POINT('Origin',(0.,0.,-1.47904511860479));
#11178=CARTESIAN_POINT('',(-1.99740252611268,-0.000992144320337381,13.3209548813952));
#11179=CARTESIAN_POINT('',(-1.9955844561164,0.00173554905423284,13.4790451186048));
#11180=CARTESIAN_POINT('',(-1.99475,4.03981020633857E-13,-1.47904511860479));
#11181=CARTESIAN_POINT('Ctrl Pts',(-1.99740252611268,-0.000992144320337198,
13.3209548813952));
#11182=CARTESIAN_POINT('Ctrl Pts',(-1.99774913123626,-0.0577895479995564,
13.3245938414828));
#11183=CARTESIAN_POINT('Ctrl Pts',(-1.96979972317684,-0.774830503751046,
13.3705562039884));
#11184=CARTESIAN_POINT('Ctrl Pts',(-1.10495101849633,-2.08242159422195,
13.4588419689119));
#11185=CARTESIAN_POINT('Ctrl Pts',(1.14957607715301,-2.05812324514239,13.5858121761658));
#11186=CARTESIAN_POINT('Ctrl Pts',(2.35255856756512,-0.151210566872388,
13.7127823834197));
#11187=CARTESIAN_POINT('Ctrl Pts',(1.40359972987109,1.894018016721,13.8397525906736));
#11188=CARTESIAN_POINT('Ctrl Pts',(-0.829265195633706,2.20674323034388,
13.9667227979275));
#11189=CARTESIAN_POINT('Ctrl Pts',(-1.91765995199167,0.947432563273637,
14.0604568948347));
#11190=CARTESIAN_POINT('Ctrl Pts',(-1.99642703549267,0.144054836087643,
14.1118675893239));
#11191=CARTESIAN_POINT('Ctrl Pts',(-1.99511464393632,0.00179586406614349,
14.1209548813952));
#11192=CARTESIAN_POINT('Ctrl Pts',(-1.9955844561164,0.00173554905423281,
13.4790451186048));
#11193=CARTESIAN_POINT('Ctrl Pts',(-1.9906881467987,-0.533933096035126,
13.5132835745814));
#11194=CARTESIAN_POINT('Ctrl Pts',(-1.4923926878599,-1.74004025674718,13.5898611371993));
#11195=CARTESIAN_POINT('Ctrl Pts',(0.545581575104675,-2.2937145738163,13.7087778064586));
#11196=CARTESIAN_POINT('Ctrl Pts',(2.22298781706136,-0.785564107140691,
13.8357951263826));
#11197=CARTESIAN_POINT('Ctrl Pts',(1.86559217928514,1.44164892460722,13.9628124463066));
#11198=CARTESIAN_POINT('Ctrl Pts',(-0.199464851904689,2.34925511047346,
14.0898297662307));
#11199=CARTESIAN_POINT('Ctrl Pts',(-1.76172155469051,1.31788471912336,14.1952406569967));
#11200=CARTESIAN_POINT('Ctrl Pts',(-1.99164750753333,0.326174945926526,
14.2583124411214));
#11201=CARTESIAN_POINT('Ctrl Pts',(-1.99148314676551,0.000112721033546474,
14.2790451186048));
#11202=CARTESIAN_POINT('Origin',(0.,0.,-1.47904511860479));
#11203=CARTESIAN_POINT('',(-1.9921588650168,-0.00114591747005889,12.5209548813952));
#11204=CARTESIAN_POINT('',(-1.99710797193854,-0.00119562967828307,12.6790451186048));
#11205=CARTESIAN_POINT('',(-1.99475,4.03981020633857E-13,-1.47904511860479));
#11206=CARTESIAN_POINT('Ctrl Pts',(-1.9921588650168,-0.00114591747005909,
12.5209548813952));
#11207=CARTESIAN_POINT('Ctrl Pts',(-1.99350475755727,-0.25830313556317,
12.5373200936417));
#11208=CARTESIAN_POINT('Ctrl Pts',(-1.82781441796359,-1.17884773168539,
12.5960087083062));
#11209=CARTESIAN_POINT('Ctrl Pts',(-0.440537590706227,-2.31588494544368,
12.6970207253886));
#11210=CARTESIAN_POINT('Ctrl Pts',(1.70621353334662,-1.62672426304606,12.8239909326425));
#11211=CARTESIAN_POINT('Ctrl Pts',(2.29225051935244,0.550439829487665,12.9509611398964));
#11212=CARTESIAN_POINT('Ctrl Pts',(0.781511384680127,2.22410350590373,13.0779313471503));
#11213=CARTESIAN_POINT('Ctrl Pts',(-1.3803090509661,1.87366660161095,13.2012625943166));
#11214=CARTESIAN_POINT('Ctrl Pts',(-1.99371789490167,0.602800102433931,
13.2822704390649));
#11215=CARTESIAN_POINT('Ctrl Pts',(-1.99740252611268,-0.000992144320337198,
13.3209548813952));
#11216=CARTESIAN_POINT('Ctrl Pts',(-1.99710797193854,-0.00119562967828295,
12.6790451186048));
#11217=CARTESIAN_POINT('Ctrl Pts',(-1.99760917397881,-0.0719494836075869,
12.6835764947587));
#11218=CARTESIAN_POINT('Ctrl Pts',(-1.96208750924084,-0.803286251661634,
12.7304469775539));
#11219=CARTESIAN_POINT('Ctrl Pts',(-1.06027625346291,-2.10584901347975,
12.8196565669905));
#11220=CARTESIAN_POINT('Ctrl Pts',(1.19424884442458,-2.03286878544129,12.9466738869145));
#11221=CARTESIAN_POINT('Ctrl Pts',(2.35562364483704,-0.0991112764303932,
13.0736912068385));
#11222=CARTESIAN_POINT('Ctrl Pts',(1.36078895832842,1.92536729278402,13.2007085267625));
#11223=CARTESIAN_POINT('Ctrl Pts',(-0.879637768350177,2.18746958783955,
13.3277258466866));
#11224=CARTESIAN_POINT('Ctrl Pts',(-1.92800865020163,0.916362008260045,
13.420504710634));
#11225=CARTESIAN_POINT('Ctrl Pts',(-1.99674289887317,0.12847212178069,13.4709444679401));
#11226=CARTESIAN_POINT('Ctrl Pts',(-1.9955844561164,0.00173554905423281,
13.4790451186048));
#11227=CARTESIAN_POINT('Origin',(0.,0.,-1.47904511860479));
#11228=CARTESIAN_POINT('',(-1.99323815944991,0.00164697314138954,11.7209548813952));
#11229=CARTESIAN_POINT('',(-1.99195362472057,-0.000981272968664654,11.8790451186048));
#11230=CARTESIAN_POINT('',(-1.99475,4.03981020633857E-13,-1.47904511860479));
#11231=CARTESIAN_POINT('Ctrl Pts',(-1.99323815944991,0.00164697314138934,
11.7209548813952));
#11232=CARTESIAN_POINT('Ctrl Pts',(-1.98967599032796,-0.454863659793869,
11.7500463458006));
#11233=CARTESIAN_POINT('Ctrl Pts',(-1.6073406180934,-1.58091626896194,11.821461212624));
#11234=CARTESIAN_POINT('Ctrl Pts',(0.263190068058092,-2.34267527357795,
11.9351994818653));
#11235=CARTESIAN_POINT('Ctrl Pts',(2.11058595164912,-1.05015398397536,12.0621696891192));
#11236=CARTESIAN_POINT('Ctrl Pts',(2.0273786194508,1.20296815533566,12.1891398963731));
#11237=CARTESIAN_POINT('Ctrl Pts',(0.0896797991062791,2.35570668441345,
12.316110103627));
#11238=CARTESIAN_POINT('Ctrl Pts',(-1.66972777748032,1.4827828112436,12.4267150986343));
#11239=CARTESIAN_POINT('Ctrl Pts',(-1.99002403572222,0.406751998589953,
12.4949966912238));
#11240=CARTESIAN_POINT('Ctrl Pts',(-1.9921588650168,-0.00114591747005909,
12.5209548813952));
#11241=CARTESIAN_POINT('Ctrl Pts',(-1.99195362472057,-0.000981272968664897,
11.8790451186048));
#11242=CARTESIAN_POINT('Ctrl Pts',(-1.99315423945754,-0.270750376731748,
11.8962085215773));
#11243=CARTESIAN_POINT('Ctrl Pts',(-1.81641900129272,-1.20448536032894,
11.9557110311912));
#11244=CARTESIAN_POINT('Ctrl Pts',(-0.396097208116597,-2.32419723839291,
12.0575526474464));
#11245=CARTESIAN_POINT('Ctrl Pts',(1.737900288011,-1.59326344028923,12.1845699673704));
#11246=CARTESIAN_POINT('Ctrl Pts',(2.28111858791796,0.596056867325744,12.3115872872944));
#11247=CARTESIAN_POINT('Ctrl Pts',(0.736325268973554,2.23977920775732,12.4386046072184));
#11248=CARTESIAN_POINT('Ctrl Pts',(-1.40330431850088,1.84782993570273,12.5610905509886));
#11249=CARTESIAN_POINT('Ctrl Pts',(-1.99292617130783,0.589142172669957,
12.6412373881174));
#11250=CARTESIAN_POINT('Ctrl Pts',(-1.99710797193854,-0.00119562967828295,
12.6790451186048));
#11251=CARTESIAN_POINT('Origin',(0.,0.,-1.47904511860479));
#11252=CARTESIAN_POINT('',(-1.99800253719316,0.00014696211896244,10.9209548813952));
#11253=CARTESIAN_POINT('',(-1.99352514341734,0.00171980163322982,11.0790451186048));
#11254=CARTESIAN_POINT('',(-1.99475,4.03981020633857E-13,-1.47904511860479));
#11255=CARTESIAN_POINT('Ctrl Pts',(-1.99800253719316,0.00014696211896245,
10.9209548813952));
#11256=CARTESIAN_POINT('Ctrl Pts',(-1.99731048143793,-0.652028054488447,
10.9627725979595));
#11257=CARTESIAN_POINT('Ctrl Pts',(-1.29377835363174,-1.96554537055817,
11.0469137169418));
#11258=CARTESIAN_POINT('Ctrl Pts',(0.943430253008483,-2.16040176982576,
11.173378238342));
#11259=CARTESIAN_POINT('Ctrl Pts',(2.32660653495589,-0.379866398696293,
11.3003484455959));
#11260=CARTESIAN_POINT('Ctrl Pts',(1.58158043085374,1.74814181063735,11.4273186528497));
#11261=CARTESIAN_POINT('Ctrl Pts',(-0.610154945358331,2.27708308851757,
11.5542888601037));
#11262=CARTESIAN_POINT('Ctrl Pts',(-1.86947320797437,1.07916638007941,11.6521676029521));
#11263=CARTESIAN_POINT('Ctrl Pts',(-1.99485837355653,0.209285898184941,
11.7077229433827));
#11264=CARTESIAN_POINT('Ctrl Pts',(-1.99323815944991,0.00164697314138934,
11.7209548813952));
#11265=CARTESIAN_POINT('Ctrl Pts',(-1.99352514341734,0.00171980163322982,
11.0790451186048));
#11266=CARTESIAN_POINT('Ctrl Pts',(-1.98967826936081,-0.465667208835488,
11.1088405483959));
#11267=CARTESIAN_POINT('Ctrl Pts',(-1.59248298847649,-1.60309637919185,
11.1809750848285));
#11268=CARTESIAN_POINT('Ctrl Pts',(0.302912497167387,-2.33816804791504,
11.2954487279023));
#11269=CARTESIAN_POINT('Ctrl Pts',(2.12873011938496,-1.01355507006492,11.4224660478263));
#11270=CARTESIAN_POINT('Ctrl Pts',(2.00602422063487,1.2388109732551,11.5494833677503));
#11271=CARTESIAN_POINT('Ctrl Pts',(0.0471130923241888,2.35723697530873,
11.6765006876744));
#11272=CARTESIAN_POINT('Ctrl Pts',(-1.68439473653372,1.45840831064242,11.7863546046258));
#11273=CARTESIAN_POINT('Ctrl Pts',(-1.99019253335153,0.394722715698714,
11.853869414936));
#11274=CARTESIAN_POINT('Ctrl Pts',(-1.99195362472057,-0.000981272968664897,
11.8790451186048));
#11275=CARTESIAN_POINT('Origin',(0.,0.,-1.47904511860479));
#11276=CARTESIAN_POINT('',(-1.99366456530849,-0.00174269800029035,10.1209548813952));
#11277=CARTESIAN_POINT('',(-1.99802112857236,-2.57504959200183E-5,10.2790451186048));
#11278=CARTESIAN_POINT('',(-1.99475,4.03981020633857E-13,-1.47904511860479));
#11279=CARTESIAN_POINT('Ctrl Pts',(-1.99366456530849,-0.00174269800029027,
10.1209548813952));
#11280=CARTESIAN_POINT('Ctrl Pts',(-1.99527275468271,-0.193407171486628,
10.1331754477005));
#11281=CARTESIAN_POINT('Ctrl Pts',(-1.88194262316761,-1.04699937041106,
10.1877194164236));
#11282=CARTESIAN_POINT('Ctrl Pts',(-0.664239202615746,-2.26189803728336,
10.2845867875648));
#11283=CARTESIAN_POINT('Ctrl Pts',(1.53947731651516,-1.78533079324062,10.4115569948187));
#11284=CARTESIAN_POINT('Ctrl Pts',(2.33499728455247,0.32432102998492,10.5385272020725));
#11285=CARTESIAN_POINT('Ctrl Pts',(0.994639648129273,2.13730868611139,10.6654974093264));
#11286=CARTESIAN_POINT('Ctrl Pts',(-1.25553855339793,1.9952492050592,10.7924676165803));
#11287=CARTESIAN_POINT('Ctrl Pts',(-1.99439780105699,0.675973613661738,
10.8776201072699));
#11288=CARTESIAN_POINT('Ctrl Pts',(-1.99801090596205,0.00803346829660538,
10.9204491955416));
#11289=CARTESIAN_POINT('Ctrl Pts',(-1.99800253719316,0.00014696211896245,
10.9209548813952));
#11290=CARTESIAN_POINT('Ctrl Pts',(-1.99802112857236,-2.57504959202544E-5,
10.2790451186048));
#11291=CARTESIAN_POINT('Ctrl Pts',(-1.99802139127224,-0.0014035926386325,
10.2791334685732));
#11292=CARTESIAN_POINT('Ctrl Pts',(-1.997396130801,-0.66307124280884,10.3215609251831));
#11293=CARTESIAN_POINT('Ctrl Pts',(-1.27452282778516,-1.98352649659275,
10.4063274884342));
#11294=CARTESIAN_POINT('Ctrl Pts',(0.975285705239301,-2.14653292413298,
10.5333448083582));
#11295=CARTESIAN_POINT('Ctrl Pts',(2.33237086341372,-0.344720113613569,
10.6603621282822));
#11296=CARTESIAN_POINT('Ctrl Pts',(1.5545308633467,1.77263069930924,10.7873794482062));
#11297=CARTESIAN_POINT('Ctrl Pts',(-0.646241956488163,2.2674119905534,10.9143967681303));
#11298=CARTESIAN_POINT('Ctrl Pts',(-1.87798874059562,1.0575211530769,11.0116186582631));
#11299=CARTESIAN_POINT('Ctrl Pts',(-1.99514465169048,0.19848660997858,11.0665014417546));
#11300=CARTESIAN_POINT('Ctrl Pts',(-1.99352514341734,0.00171980163322982,
11.0790451186048));
#11301=CARTESIAN_POINT('Origin',(0.,0.,-1.47904511860479));
#11302=CARTESIAN_POINT('',(-1.99190842477769,0.000930945868489363,9.32095488139522));
#11303=CARTESIAN_POINT('',(-1.99344998719875,-0.00170364987860938,9.47904511860478));
#11304=CARTESIAN_POINT('',(-1.99475,4.03981020633857E-13,-1.47904511860479));
#11305=CARTESIAN_POINT('Ctrl Pts',(-1.99190842477769,0.000930945868489394,
9.32095488139522));
#11306=CARTESIAN_POINT('Ctrl Pts',(-1.99025409107239,-0.391198045614882,
9.34590169985934));
#11307=CARTESIAN_POINT('Ctrl Pts',(-1.68869165330305,-1.45093925392043,
9.41317192074142));
#11308=CARTESIAN_POINT('Ctrl Pts',(0.0335234320998379,-2.35717471326548,
9.52276554404145));
#11309=CARTESIAN_POINT('Ctrl Pts',(1.99813913054961,-1.25093423661054,9.64973575129535));
#11310=CARTESIAN_POINT('Ctrl Pts',(2.13500939744307,0.999565566727712,9.77670595854921));
#11311=CARTESIAN_POINT('Ctrl Pts',(0.318935741240959,2.33573894995075,9.90367616580313));
#11312=CARTESIAN_POINT('Ctrl Pts',(-1.58600439547375,1.61239114596766,10.0184258067518));
#11313=CARTESIAN_POINT('Ctrl Pts',(-1.98970312359121,0.470383068506138,
10.0908520452825));
#11314=CARTESIAN_POINT('Ctrl Pts',(-1.99366456530849,-0.00174269800029027,
10.1209548813952));
#11315=CARTESIAN_POINT('Ctrl Pts',(-1.99344998719875,-0.0017036498786095,
9.47904511860478));
#11316=CARTESIAN_POINT('Ctrl Pts',(-1.99507240931094,-0.201261304212527,
9.49176549539188));
#11317=CARTESIAN_POINT('Ctrl Pts',(-1.87581742430337,-1.06314114597083,
9.54682497882032));
#11318=CARTESIAN_POINT('Ctrl Pts',(-0.636796252956758,-2.27008289131724,
9.64422356889009));
#11319=CARTESIAN_POINT('Ctrl Pts',(1.5618975293753,-1.76614323002478,9.77124088881411));
#11320=CARTESIAN_POINT('Ctrl Pts',(2.33091544739048,0.354427677174692,9.89825820873813));
#11321=CARTESIAN_POINT('Ctrl Pts',(0.966340415661779,2.15057480741536,10.0252755286621));
#11322=CARTESIAN_POINT('Ctrl Pts',(-1.28120553730588,1.97832287734288,10.1522044986177));
#11323=CARTESIAN_POINT('Ctrl Pts',(-1.99789550012917,0.65888646097121,10.2367943619319));
#11324=CARTESIAN_POINT('Ctrl Pts',(-1.99802112857236,-2.57504959202544E-5,
10.2790451186048));
#11325=CARTESIAN_POINT('Origin',(0.,0.,-1.47904511860479));
#11326=CARTESIAN_POINT('',(-1.99706026989319,0.00121875038140872,8.52095488139522));
#11327=CARTESIAN_POINT('',(-1.991995621869,0.00101962588792096,8.67904511860479));
#11328=CARTESIAN_POINT('',(-1.99475,4.03981020633857E-13,-1.47904511860479));
#11329=CARTESIAN_POINT('Ctrl Pts',(-1.99706026989319,0.00121875038140875,
8.52095488139522));
#11330=CARTESIAN_POINT('Ctrl Pts',(-1.99282941906458,-0.587053347272268,
8.55862795201823));
#11331=CARTESIAN_POINT('Ctrl Pts',(-1.40690779658877,-1.84354047944384,
8.63862442505921));
#11332=CARTESIAN_POINT('Ctrl Pts',(0.72829438578655,-2.24209360575996,8.76094430051814));
#11333=CARTESIAN_POINT('Ctrl Pts',(2.27848403144356,-0.604902444874099,
8.88791450777203));
#11334=CARTESIAN_POINT('Ctrl Pts',(1.74449009064557,1.58560738299156,9.01488471502591));
#11335=CARTESIAN_POINT('Ctrl Pts',(-0.385230466394427,2.32572438975891,
9.1418549222798));
#11336=CARTESIAN_POINT('Ctrl Pts',(-1.81336359917182,1.21101525639225,9.24387831106957));
#11337=CARTESIAN_POINT('Ctrl Pts',(-1.99306074280009,0.274066470185944,
9.30357829744137));
#11338=CARTESIAN_POINT('Ctrl Pts',(-1.99190842477769,0.000930945868489394,
9.32095488139522));
#11339=CARTESIAN_POINT('Ctrl Pts',(-1.991995621869,0.00101962588792109,
8.67904511860479));
#11340=CARTESIAN_POINT('Ctrl Pts',(-1.99015055945641,-0.397440654073741,
8.70439752221052));
#11341=CARTESIAN_POINT('Ctrl Pts',(-1.68109935098533,-1.46397429262776,
8.77208903245758));
#11342=CARTESIAN_POINT('Ctrl Pts',(0.0569267623458949,-2.35702039553327,
8.882119649346));
#11343=CARTESIAN_POINT('Ctrl Pts',(2.01116447809095,-1.23044839115509,9.00913696927002));
#11344=CARTESIAN_POINT('Ctrl Pts',(2.12449185277921,1.02240900265292,9.13615428919402));
#11345=CARTESIAN_POINT('Ctrl Pts',(0.293175184736282,2.33940892369971,9.26317160911806));
#11346=CARTESIAN_POINT('Ctrl Pts',(-1.59622253240353,1.59759918753759,9.37746855225496));
#11347=CARTESIAN_POINT('Ctrl Pts',(-1.98967226244618,0.462955876563709,
9.44942638875054));
#11348=CARTESIAN_POINT('Ctrl Pts',(-1.99344998719875,-0.0017036498786095,
9.47904511860478));
#11349=CARTESIAN_POINT('Origin',(0.,0.,-1.47904511860479));
#11350=CARTESIAN_POINT('',(-1.99559319474839,-0.00173033593146375,7.72095488139522));
#11351=CARTESIAN_POINT('',(-1.99717077118997,0.00115749627489468,7.87904511860478));
#11352=CARTESIAN_POINT('',(-1.99475,4.03981020633857E-13,-1.47904511860479));
#11353=CARTESIAN_POINT('Ctrl Pts',(-1.99559319474839,-0.00173033593146354,
7.72095488139522));
#11354=CARTESIAN_POINT('Ctrl Pts',(-1.99674614175328,-0.128078601059412,
7.72903080175916));
#11355=CARTESIAN_POINT('Ctrl Pts',(-1.92827410556723,-0.91533394716936,
7.77943012454107));
#11356=CARTESIAN_POINT('Ctrl Pts',(-0.8816112114347,-2.18635727209223,7.87215284974095));
#11357=CARTESIAN_POINT('Ctrl Pts',(1.35807126336241,-1.92692472426588,7.99912305699481));
#11358=CARTESIAN_POINT('Ctrl Pts',(2.35549362254096,0.0951117423181714,
8.12609326424872));
#11359=CARTESIAN_POINT('Ctrl Pts',(1.19828988895336,2.03014723391927,8.25306347150259));
#11360=CARTESIAN_POINT('Ctrl Pts',(-1.05501813323409,2.10815871980864,8.38003367875648));
#11361=CARTESIAN_POINT('Ctrl Pts',(-1.96103960865442,0.806807176619804,
8.46933081538736));
#11362=CARTESIAN_POINT('Ctrl Pts',(-1.99758252252093,0.0738345577621752,
8.51630454960027));
#11363=CARTESIAN_POINT('Ctrl Pts',(-1.99706026989319,0.00121875038140875,
8.52095488139522));
#11364=CARTESIAN_POINT('Ctrl Pts',(-1.99717077118997,0.00115749627489461,
7.87904511860478));
#11365=CARTESIAN_POINT('Ctrl Pts',(-1.9930751220383,-0.591890300141836,
7.91702954902914));
#11366=CARTESIAN_POINT('Ctrl Pts',(-1.39868792096064,-1.85310383721029,
7.99735308609486));
#11367=CARTESIAN_POINT('Ctrl Pts',(0.745643944080418,-2.23669419230417,
8.1200157298019));
#11368=CARTESIAN_POINT('Ctrl Pts',(2.28358043018348,-0.586554532941333,
8.24703304972591));
#11369=CARTESIAN_POINT('Ctrl Pts',(1.73125186121253,1.60048517465147,8.37405036964994));
#11370=CARTESIAN_POINT('Ctrl Pts',(-0.405770296472382,2.32252799073159,
8.50106768957393));
#11371=CARTESIAN_POINT('Ctrl Pts',(-1.81896177685869,1.19886546994113,8.60273260589224));
#11372=CARTESIAN_POINT('Ctrl Pts',(-1.99323185681431,0.267997327586453,
8.66205841556918));
#11373=CARTESIAN_POINT('Ctrl Pts',(-1.991995621869,0.00101962588792109,
8.67904511860479));
#11374=CARTESIAN_POINT('Origin',(0.,0.,-1.47904511860479));
#11375=CARTESIAN_POINT('',(-1.99148666886423,-9.26359632818219E-5,6.92095488139522));
#11376=CARTESIAN_POINT('',(-1.995501255299,-0.00174979995018254,7.07904511860477));
#11377=CARTESIAN_POINT('',(-1.99475,4.03981020633857E-13,-1.47904511860479));
#11378=CARTESIAN_POINT('Ctrl Pts',(-1.99148666886423,-9.26359632821144E-5,
6.92095488139522));
#11379=CARTESIAN_POINT('Ctrl Pts',(-1.99162228600117,-0.327246622674157,
6.94175705391806));
#11380=CARTESIAN_POINT('Ctrl Pts',(-1.76063412440334,-1.31983678912773,
7.00488262885886));
#11381=CARTESIAN_POINT('Ctrl Pts',(-0.1964626520611,-2.34921239476192,7.11033160621761));
#11382=CARTESIAN_POINT('Ctrl Pts',(1.86665183793563,-1.43979420935406,7.23730181347151));
#11383=CARTESIAN_POINT('Ctrl Pts',(2.22229545319173,0.786638015914119,7.36427202072539));
#11384=CARTESIAN_POINT('Ctrl Pts',(0.54515251217721,2.29351372087127,7.49124222797928));
#11385=CARTESIAN_POINT('Ctrl Pts',(-1.49226254770249,1.74005184336971,7.61013651486923));
#11386=CARTESIAN_POINT('Ctrl Pts',(-1.99070390286835,0.534073603127432,
7.6867073993412));
#11387=CARTESIAN_POINT('Ctrl Pts',(-1.99559319474839,-0.00173033593146354,
7.72095488139522));
#11388=CARTESIAN_POINT('Ctrl Pts',(-1.995501255299,-0.00174979995018244,
7.07904511860477));
#11389=CARTESIAN_POINT('Ctrl Pts',(-1.99668912531657,-0.131264798487339,
7.08732246920644));
#11390=CARTESIAN_POINT('Ctrl Pts',(-1.92618348836682,-0.921968576958176,
7.13793892644944));
#11391=CARTESIAN_POINT('Ctrl Pts',(-0.870522872770069,-2.19111289741426,
7.23089449033379));
#11392=CARTESIAN_POINT('Ctrl Pts',(1.3687932043082,-1.91968512133389,7.3579118102578));
#11393=CARTESIAN_POINT('Ctrl Pts',(2.35519059073263,0.108917778877055,7.48492913018183));
#11394=CARTESIAN_POINT('Ctrl Pts',(1.18577488435873,2.03782328106611,7.61194645010582));
#11395=CARTESIAN_POINT('Ctrl Pts',(-1.06903451833457,2.10141642704157,7.73896377002986));
#11396=CARTESIAN_POINT('Ctrl Pts',(-1.96363940588376,0.797697806598223,
7.8279966595295));
#11397=CARTESIAN_POINT('Ctrl Pts',(-1.99764031162416,0.0691466988436851,
7.87469044238781));
#11398=CARTESIAN_POINT('Ctrl Pts',(-1.99717077118997,0.00115749627489461,
7.87904511860478));
#11399=CARTESIAN_POINT('Origin',(0.,0.,-1.47904511860479));
#11400=CARTESIAN_POINT('',(-1.99525355952187,0.00178111082825299,6.12095488139522));
#11401=CARTESIAN_POINT('',(-1.99147941923728,-6.71563141235731E-5,6.27904511860477));
#11402=CARTESIAN_POINT('',(-1.99475,4.03981020633857E-13,-1.47904511860479));
#11403=CARTESIAN_POINT('Ctrl Pts',(-1.99525355952187,0.00178111082825295,
6.12095488139522));
#11404=CARTESIAN_POINT('Ctrl Pts',(-1.99041683713606,-0.523003000897414,
6.15448330607696));
#11405=CARTESIAN_POINT('Ctrl Pts',(-1.50926405869879,-1.71807636877895,
6.23033513317666));
#11406=CARTESIAN_POINT('Ctrl Pts',(0.506218527102226,-2.3024203031107,6.3485103626943));
#11407=CARTESIAN_POINT('Ctrl Pts',(2.20864962127088,-0.824174313976057,
6.4754805699482));
#11408=CARTESIAN_POINT('Ctrl Pts',(1.8907763264874,1.40796354091743,6.60245077720207));
#11409=CARTESIAN_POINT('Ctrl Pts',(-0.156635087036384,2.35220362614869,
6.72942098445597));
#11410=CARTESIAN_POINT('Ctrl Pts',(-1.74880480475359,1.34263767884721,6.835589019187));
#11411=CARTESIAN_POINT('Ctrl Pts',(-1.99134636392355,0.338369904494061,
6.89943365150009));
#11412=CARTESIAN_POINT('Ctrl Pts',(-1.99148666886423,-9.26359632821144E-5,
6.92095488139522));
#11413=CARTESIAN_POINT('Ctrl Pts',(-1.99147941923728,-6.7156314123816E-5,
6.27904511860477));
#11414=CARTESIAN_POINT('Ctrl Pts',(-1.99157816546678,-0.32890987126841,
6.29995449602507));
#11415=CARTESIAN_POINT('Ctrl Pts',(-1.75884540947334,-1.32349005241169,
6.3632029800867));
#11416=CARTESIAN_POINT('Ctrl Pts',(-0.189682276366992,-2.35006519808776,
6.46879057078969));
#11417=CARTESIAN_POINT('Ctrl Pts',(1.87157814575952,-1.43386925678263,6.5958078907137));
#11418=CARTESIAN_POINT('Ctrl Pts',(2.21969794703782,0.794812446522514,6.72282521063772));
#11419=CARTESIAN_POINT('Ctrl Pts',(0.536027236282382,2.29596615898285,6.84984253056173));
#11420=CARTESIAN_POINT('Ctrl Pts',(-1.4965994031063,1.73464708792947,6.96858249988409));
#11421=CARTESIAN_POINT('Ctrl Pts',(-1.99061310440479,0.531211590227516,
7.0449833625651));
#11422=CARTESIAN_POINT('Ctrl Pts',(-1.995501255299,-0.00174979995018244,
7.07904511860477));
#11423=CARTESIAN_POINT('Origin',(0.,0.,-1.47904511860479));
#11424=CARTESIAN_POINT('',(-1.99730956637596,-0.00106064172337803,5.32095488139522));
#11425=CARTESIAN_POINT('',(-1.99525472473012,0.0017845551702237,5.47904511860478));
#11426=CARTESIAN_POINT('',(-1.99475,4.03981020633857E-13,-1.47904511860479));
#11427=CARTESIAN_POINT('Ctrl Pts',(-1.99730956637596,-0.00106064172337789,
5.32095488139522));
#11428=CARTESIAN_POINT('Ctrl Pts',(-1.99770497237211,-0.0624280686180993,
5.32488615581789));
#11429=CARTESIAN_POINT('Ctrl Pts',(-1.96730967016266,-0.784069391199876,
5.37114083265851));
#11430=CARTESIAN_POINT('Ctrl Pts',(-1.09058225712671,-2.08998248552431,
5.4597189119171));
#11431=CARTESIAN_POINT('Ctrl Pts',(1.16372401066593,-2.05015679311548,5.58668911917098));
#11432=CARTESIAN_POINT('Ctrl Pts',(2.35354422162328,-0.13500387483914,5.71365932642487));
#11433=CARTESIAN_POINT('Ctrl Pts',(1.39052150324245,1.903640301732,5.84062953367876));
#11434=CARTESIAN_POINT('Ctrl Pts',(-0.844444337704187,2.20097937515945,
5.96759974093265));
#11435=CARTESIAN_POINT('Ctrl Pts',(-1.92077276943005,0.938152829706547,
6.0610415235048));
#11436=CARTESIAN_POINT('Ctrl Pts',(-1.99652229988481,0.139439370134114,
6.11215990365899));
#11437=CARTESIAN_POINT('Ctrl Pts',(-1.99525355952187,0.00178111082825295,
6.12095488139522));
#11438=CARTESIAN_POINT('Ctrl Pts',(-1.99525472473012,0.0017845551702237,
5.47904511860478));
#11439=CARTESIAN_POINT('Ctrl Pts',(-1.99041023735962,-0.523201771333229,
5.51258652284371));
#11440=CARTESIAN_POINT('Ctrl Pts',(-1.50887731739964,-1.71873699628024,
5.58846703372397));
#11441=CARTESIAN_POINT('Ctrl Pts',(0.507837960106644,-2.30236539400368,
5.70668665124559));
#11442=CARTESIAN_POINT('Ctrl Pts',(2.20978656254498,-0.821966635105482,
5.83370397116961));
#11443=CARTESIAN_POINT('Ctrl Pts',(1.88901699407625,1.41081557877779,5.96072129109363));
#11444=CARTESIAN_POINT('Ctrl Pts',(-0.160855766453599,2.35221411092393,
6.08773861101763));
#11445=CARTESIAN_POINT('Ctrl Pts',(-1.75028149311093,1.3399904347984,6.19384655352136));
#11446=CARTESIAN_POINT('Ctrl Pts',(-1.99137821560422,0.336959154710372,
6.25761538938374));
#11447=CARTESIAN_POINT('Ctrl Pts',(-1.99147941923728,-6.7156314123816E-5,
6.27904511860477));
#11448=CARTESIAN_POINT('Origin',(0.,0.,-1.47904511860479));
#11449=CARTESIAN_POINT('',(-1.99208101634156,-0.00108597322356468,4.52095488139522));
#11450=CARTESIAN_POINT('',(-1.99734577058445,-0.00103987188155213,4.67904511860477));
#11451=CARTESIAN_POINT('',(-1.99475,4.03981020633857E-13,-1.47904511860479));
#11452=CARTESIAN_POINT('Ctrl Pts',(-1.99208101634156,-0.00108597322356466,
4.52095488139522));
#11453=CARTESIAN_POINT('Ctrl Pts',(-1.99337623546945,-0.262862144141555,
4.53761240797678));
#11454=CARTESIAN_POINT('Ctrl Pts',(-1.82368896996318,-1.18814603783072,
4.5965933369763));
#11455=CARTESIAN_POINT('Ctrl Pts',(-0.424576623578355,-2.31886419181245,
4.69789766839378));
#11456=CARTESIAN_POINT('Ctrl Pts',(1.71737702962559,-1.61493423626845,4.82486787564767));
#11457=CARTESIAN_POINT('Ctrl Pts',(2.28840502897144,0.566214511237573,4.95183808290156));
#11458=CARTESIAN_POINT('Ctrl Pts',(0.766174469238656,2.22943336568846,5.07880829015544));
#11459=CARTESIAN_POINT('Ctrl Pts',(-1.3880630675663,1.86498122595536,5.20184722298667));
#11460=CARTESIAN_POINT('Ctrl Pts',(-1.99344810162381,0.59824275325246,5.28256275339993));
#11461=CARTESIAN_POINT('Ctrl Pts',(-1.99730956637596,-0.00106064172337789,
5.32095488139522));
#11462=CARTESIAN_POINT('Ctrl Pts',(-1.99734577058445,-0.00103987188155228,
4.67904511860477));
#11463=CARTESIAN_POINT('Ctrl Pts',(-1.99772514422821,-0.0608910454152072,
4.682879443021));
#11464=CARTESIAN_POINT('Ctrl Pts',(-1.96813705138938,-0.781246353584555,
4.72905287407857));
#11465=CARTESIAN_POINT('Ctrl Pts',(-1.09471794236404,-2.08815191686271,
4.81756541177748));
#11466=CARTESIAN_POINT('Ctrl Pts',(1.16070165538423,-2.05220794960434,4.94458273170149));
#11467=CARTESIAN_POINT('Ctrl Pts',(2.35367822395426,-0.13778468461515,5.07160005162551));
#11468=CARTESIAN_POINT('Ctrl Pts',(1.3922260378406,1.90275917046527,5.19861737154953));
#11469=CARTESIAN_POINT('Ctrl Pts',(-0.843593977493136,2.20162099426043,
5.32563469147353));
#11470=CARTESIAN_POINT('Ctrl Pts',(-1.9207312990425,0.938483163076661,5.41911060715863));
#11471=CARTESIAN_POINT('Ctrl Pts',(-1.99652540373551,0.13948521412321,5.47024741620237));
#11472=CARTESIAN_POINT('Ctrl Pts',(-1.99525472473012,0.0017845551702237,
5.47904511860478));
#11473=CARTESIAN_POINT('Origin',(0.,0.,-1.47904511860479));
#11474=CARTESIAN_POINT('',(-1.99335826076814,0.00167831318840674,3.72095488139522));
#11475=CARTESIAN_POINT('',(-1.99212878278616,-0.00112883914168277,3.87904511860477));
#11476=CARTESIAN_POINT('',(-1.99475,4.03981020633857E-13,-1.47904511860479));
#11477=CARTESIAN_POINT('Ctrl Pts',(-1.99335826076814,0.00167831318840671,
3.72095488139522));
#11478=CARTESIAN_POINT('Ctrl Pts',(-1.98967611077165,-0.459349191220618,
3.75033866013568));
#11479=CARTESIAN_POINT('Ctrl Pts',(-1.60123477712065,-1.59002462297684,
3.82204584129409));
#11480=CARTESIAN_POINT('Ctrl Pts',(0.279318860454586,-2.34080700264011,
3.93607642487046));
#11481=CARTESIAN_POINT('Ctrl Pts',(2.11776876365419,-1.03559254199705,4.06304663212436));
#11482=CARTESIAN_POINT('Ctrl Pts',(2.01904516192129,1.21690307069604,4.19001683937824));
#11483=CARTESIAN_POINT('Ctrl Pts',(0.0734528840375746,2.35626847434518,
4.31698704663213));
#11484=CARTESIAN_POINT('Ctrl Pts',(-1.67526686991482,1.47358648511445,4.42729972730445));
#11485=CARTESIAN_POINT('Ctrl Pts',(-1.99008534590667,0.402258104711046,
4.49528900555882));
#11486=CARTESIAN_POINT('Ctrl Pts',(-1.99208101634156,-0.00108597322356466,
4.52095488139522));
#11487=CARTESIAN_POINT('Ctrl Pts',(-1.99212878278616,-0.00112883914168287,
3.87904511860477));
#11488=CARTESIAN_POINT('Ctrl Pts',(-1.99346081133728,-0.25988492631503,
3.89551146983963));
#11489=CARTESIAN_POINT('Ctrl Pts',(-1.82636130136228,-1.1823140336403,3.95431692771583));
#11490=CARTESIAN_POINT('Ctrl Pts',(-0.434214441284883,-2.31737860959731,
4.05546149223338));
#11491=CARTESIAN_POINT('Ctrl Pts',(1.71149948445725,-1.62159036625522,4.18247881215739));
#11492=CARTESIAN_POINT('Ctrl Pts',(2.29060007052677,0.558513310613506,4.30949613208142));
#11493=CARTESIAN_POINT('Ctrl Pts',(0.77301020537091,2.22738434573485,4.43651345200542));
#11494=CARTESIAN_POINT('Ctrl Pts',(-1.38497920298751,1.86859714880058,4.55969644751322));
#11495=CARTESIAN_POINT('Ctrl Pts',(-1.99353605133559,0.599993361789769,
4.64054033637966));
#11496=CARTESIAN_POINT('Ctrl Pts',(-1.99734577058445,-0.00103987188155228,
4.67904511860477));
#11497=CARTESIAN_POINT('Origin',(0.,0.,-1.47904511860479));
#11498=CARTESIAN_POINT('',(-1.99801366137741,6.20784135630644E-5,2.92095488139522));
#11499=CARTESIAN_POINT('',(-1.99323413496252,0.00164975376670227,3.07904511860477));
#11500=CARTESIAN_POINT('',(-1.99475,4.03981020633857E-13,-1.47904511860479));
#11501=CARTESIAN_POINT('Ctrl Pts',(-1.99801366137741,6.20784135629766E-5,
2.92095488139522));
#11502=CARTESIAN_POINT('Ctrl Pts',(-1.9977139479877,-0.656661905859173,
2.96306491229457));
#11503=CARTESIAN_POINT('Ctrl Pts',(-1.28538422970207,-1.97399479890882,
3.04749834561188));
#11504=CARTESIAN_POINT('Ctrl Pts',(0.958287513109827,-2.15385270943036,
3.17425518134715));
#11505=CARTESIAN_POINT('Ctrl Pts',(2.32916765789381,-0.363833025997572,
3.30122538860104));
#11506=CARTESIAN_POINT('Ctrl Pts',(1.56950269631471,1.75899338684286,3.42819559585493));
#11507=CARTESIAN_POINT('Ctrl Pts',(-0.6258237459619,2.27282667370784,3.55516580310881));
#11508=CARTESIAN_POINT('Ctrl Pts',(-1.87312534234062,1.06986828966388,3.65275223162224));
#11509=CARTESIAN_POINT('Ctrl Pts',(-1.99497975525663,0.204699254256833,
3.70801525771771));
#11510=CARTESIAN_POINT('Ctrl Pts',(-1.99335826076814,0.00167831318840671,
3.72095488139522));
#11511=CARTESIAN_POINT('Ctrl Pts',(-1.99323413496252,0.00164975376670215,
3.07904511860477));
#11512=CARTESIAN_POINT('Ctrl Pts',(-1.98966787406762,-0.454971437589277,
3.10814349665827));
#11513=CARTESIAN_POINT('Ctrl Pts',(-1.60712975765151,-1.5813915076858,3.1795809813531));
#11514=CARTESIAN_POINT('Ctrl Pts',(0.264471544354857,-2.34282748059378,
3.29335757268928));
#11515=CARTESIAN_POINT('Ctrl Pts',(2.11179724612446,-1.04837884014621,3.42037489261329));
#11516=CARTESIAN_POINT('Ctrl Pts',(2.02609885609852,1.2056986466197,3.54739221253732));
#11517=CARTESIAN_POINT('Ctrl Pts',(0.0858200094412126,2.35614531115273,
3.67440953246132));
#11518=CARTESIAN_POINT('Ctrl Pts',(-1.67129494903997,1.48035260045669,3.78496050115049));
#11519=CARTESIAN_POINT('Ctrl Pts',(-1.99003583284199,0.405441678994632,
3.8531723631983));
#11520=CARTESIAN_POINT('Ctrl Pts',(-1.99212878278616,-0.00112883914168287,
3.87904511860477));
#11521=CARTESIAN_POINT('Origin',(0.,0.,-1.47904511860479));
#11522=CARTESIAN_POINT('',(-1.99353828631959,-0.00171873314672716,2.12095488139522));
#11523=CARTESIAN_POINT('',(-1.99800195695475,0.000177068703322431,2.27904511860477));
#11524=CARTESIAN_POINT('',(-1.99475,4.03981020633857E-13,-1.47904511860479));
#11525=CARTESIAN_POINT('Ctrl Pts',(-1.99353828631959,-0.00171873314672709,
2.12095488139522));
#11526=CARTESIAN_POINT('Ctrl Pts',(-1.99515465902021,-0.197999298554213,
2.1334677620355));
#11527=CARTESIAN_POINT('Ctrl Pts',(-1.87838664997211,-1.05629559439167,
2.18830404509374));
#11528=CARTESIAN_POINT('Ctrl Pts',(-0.648644751766769,-2.26641924187756,
2.28546373056995));
#11529=CARTESIAN_POINT('Ctrl Pts',(1.55173715555782,-1.77468541835342,2.41243393782384));
#11530=CARTESIAN_POINT('Ctrl Pts',(2.33270816248269,0.340395505542482,2.53940414507772));
#11531=CARTESIAN_POINT('Ctrl Pts',(0.979895470300759,2.14410850487368,2.66637435233161));
#11532=CARTESIAN_POINT('Ctrl Pts',(-1.2692509317393,1.98655443822406,2.7933445595855));
#11533=CARTESIAN_POINT('Ctrl Pts',(-1.99650109561173,0.666767500964708,
2.87820473594003));
#11534=CARTESIAN_POINT('Ctrl Pts',(-1.9980151800251,0.00338969871783043,
2.9207415098766));
#11535=CARTESIAN_POINT('Ctrl Pts',(-1.99801366137741,6.20784135629766E-5,
2.92095488139522));
#11536=CARTESIAN_POINT('Ctrl Pts',(-1.99800195695475,0.000177068703322262,
2.27904511860477));
#11537=CARTESIAN_POINT('Ctrl Pts',(-1.9971755937525,-0.650636966490359,
2.3207755234769));
#11538=CARTESIAN_POINT('Ctrl Pts',(-1.29615928203765,-1.96328542074049,
2.40484503499037));
#11539=CARTESIAN_POINT('Ctrl Pts',(0.939901322271841,-2.16226069656491,
2.53125365314518));
#11540=CARTESIAN_POINT('Ctrl Pts',(2.32639490702415,-0.382978510636179,
2.6582709730692));
#11541=CARTESIAN_POINT('Ctrl Pts',(1.58343339573353,1.74686132178264,2.78528829299322));
#11542=CARTESIAN_POINT('Ctrl Pts',(-0.608916736747748,2.27771951988605,
2.91230561291723));
#11543=CARTESIAN_POINT('Ctrl Pts',(-1.8693401495715,1.07969268184623,3.01022455478775));
#11544=CARTESIAN_POINT('Ctrl Pts',(-1.99485690213174,0.209427563618705,
3.06580439001693));
#11545=CARTESIAN_POINT('Ctrl Pts',(-1.99323413496252,0.00164975376670215,
3.07904511860477));
#11546=CARTESIAN_POINT('Origin',(0.,0.,-1.47904511860479));
#11547=CARTESIAN_POINT('',(-1.99197487574581,0.000997555507514769,1.32095488139522));
#11548=CARTESIAN_POINT('',(-1.99375138711093,-0.00176081023319702,1.47904511860477));
#11549=CARTESIAN_POINT('',(-1.99475,4.03981020633857E-13,-1.47904511860479));
#11550=CARTESIAN_POINT('Ctrl Pts',(-1.99197487574581,0.000997555507514826,
1.32095488139522));
#11551=CARTESIAN_POINT('Ctrl Pts',(-1.99018227073014,-0.395693898889233,
1.34619401419439));
#11552=CARTESIAN_POINT('Ctrl Pts',(-1.68326915044115,-1.46015401124514,
1.41375654941153));
#11553=CARTESIAN_POINT('Ctrl Pts',(0.0497579841286025,-2.35688535243524,
1.52364248704663));
#11554=CARTESIAN_POINT('Ctrl Pts',(2.00670723621032,-1.23714384781738,1.65061269430052));
#11555=CARTESIAN_POINT('Ctrl Pts',(2.1280744337024,1.01424731308453,1.77758290155441));
#11556=CARTESIAN_POINT('Ctrl Pts',(0.302840850211159,2.33787982927957,1.90455310880829));
#11557=CARTESIAN_POINT('Ctrl Pts',(-1.59223214373163,1.60330557312612,2.0190104354219));
#11558=CARTESIAN_POINT('Ctrl Pts',(-1.98968746131953,0.465897496706805,
2.09114435961754));
#11559=CARTESIAN_POINT('Ctrl Pts',(-1.99353828631959,-0.00171873314672709,
2.12095488139522));
#11560=CARTESIAN_POINT('Ctrl Pts',(-1.99375138711093,-0.00176081023319709,
1.47904511860477));
#11561=CARTESIAN_POINT('Ctrl Pts',(-1.99535436761224,-0.190310974989928,
1.4910684436542));
#11562=CARTESIAN_POINT('Ctrl Pts',(-1.88430048103082,-1.04097352315297,
1.54543087534496));
#11563=CARTESIAN_POINT('Ctrl Pts',(-0.673992169187479,-2.25931816777247,
1.64213241367707));
#11564=CARTESIAN_POINT('Ctrl Pts',(1.53268116536722,-1.79155650545778,1.76914973360108));
#11565=CARTESIAN_POINT('Ctrl Pts',(2.33642193463667,0.316098985050819,1.8961670535251));
#11566=CARTESIAN_POINT('Ctrl Pts',(1.00152929412067,2.13441435022671,2.02318437344912));
#11567=CARTESIAN_POINT('Ctrl Pts',(-1.25010860812744,1.99900333994266,2.15020169337313));
#11568=CARTESIAN_POINT('Ctrl Pts',(-1.9936531346221,0.679459076978294,2.23548860842502));
#11569=CARTESIAN_POINT('Ctrl Pts',(-1.99801401072573,0.0096701866316292,
2.27843641683556));
#11570=CARTESIAN_POINT('Ctrl Pts',(-1.99800195695475,0.000177068703322262,
2.27904511860477));
#11571=CARTESIAN_POINT('Origin',(0.,0.,-1.47904511860479));
#11572=CARTESIAN_POINT('',(-1.99714087507904,0.0012938138350061,0.52095488139522));
#11573=CARTESIAN_POINT('',(-1.99183435874083,0.000880024085723324,0.679045118604771));
#11574=CARTESIAN_POINT('',(-1.99475,4.03981020633857E-13,-1.47904511860479));
#11575=CARTESIAN_POINT('Ctrl Pts',(-1.99714087507904,0.00129381383500625,
0.52095488139522));
#11576=CARTESIAN_POINT('Ctrl Pts',(-1.99304294628744,-0.591424958441748,
0.55892026635329));
#11577=CARTESIAN_POINT('Ctrl Pts',(-1.39932480947917,-1.85249014707753,
0.639209053729322));
#11578=CARTESIAN_POINT('Ctrl Pts',(0.743740789408913,-2.23690209703098,
0.761821243523316));
#11579=CARTESIAN_POINT('Ctrl Pts',(2.28258498544192,-0.589259358513722,
0.888791450777202));
#11580=CARTESIAN_POINT('Ctrl Pts',(1.73353383587625,1.59761854395386,1.01576165803109));
#11581=CARTESIAN_POINT('Ctrl Pts',(-0.401242712543095,2.32299828124824,
1.14273186528497));
#11582=CARTESIAN_POINT('Ctrl Pts',(-1.8175909465059,1.20172296388846,1.24446293973969));
#11583=CARTESIAN_POINT('Ctrl Pts',(-1.99318828302297,0.269516439112097,
1.30387061177643));
#11584=CARTESIAN_POINT('Ctrl Pts',(-1.99197487574581,0.000997555507514826,
1.32095488139522));
#11585=CARTESIAN_POINT('Ctrl Pts',(-1.99183435874083,0.00088002408572329,
0.679045118604771));
#11586=CARTESIAN_POINT('Ctrl Pts',(-1.9903216505241,-0.386707492335019,
0.703700470472832));
#11587=CARTESIAN_POINT('Ctrl Pts',(-1.69400858548477,-1.44203090012767,
0.770694928982232));
#11588=CARTESIAN_POINT('Ctrl Pts',(0.0182153715595747,-2.3576204698764,
0.88002849413297));
#11589=CARTESIAN_POINT('Ctrl Pts',(1.9906822371454,-1.26332101110348,1.00704581405699));
#11590=CARTESIAN_POINT('Ctrl Pts',(2.14099816144828,0.987384922727256,1.134063133981));
#11591=CARTESIAN_POINT('Ctrl Pts',(0.331555254300241,2.33427609427238,1.26108045390502));
#11592=CARTESIAN_POINT('Ctrl Pts',(-1.58136473144127,1.61926551238329,1.37607444877961));
#11593=CARTESIAN_POINT('Ctrl Pts',(-1.98970960943512,0.473652238186084,
1.44872933701286));
#11594=CARTESIAN_POINT('Ctrl Pts',(-1.99375138711093,-0.00176081023319709,
1.47904511860477));
#11595=CARTESIAN_POINT('Origin',(0.,0.,24.5));
#11596=CARTESIAN_POINT('',(-2.39498807124001,0.000954274581741462,24.1082520126806));
#11597=CARTESIAN_POINT('Ctrl Pts',(-0.4076525627588,1.95265126189399,24.50525));
#11598=CARTESIAN_POINT('Ctrl Pts',(-0.337699253117069,1.97023462451848,
24.5023335797628));
#11599=CARTESIAN_POINT('Ctrl Pts',(-0.266932744787586,1.98367656997238,
24.4994292108287));
#11600=CARTESIAN_POINT('Ctrl Pts',(-0.195667102851186,1.99314829867957,
24.4965325858746));
#11601=CARTESIAN_POINT('Ctrl Pts',(-0.12076554741437,2.00310326707061,24.4934881775358));
#11602=CARTESIAN_POINT('Ctrl Pts',(-0.0453118238453052,2.00867281937902,
24.4904523235171));
#11603=CARTESIAN_POINT('Ctrl Pts',(0.0303460012294243,2.00999925550285,
24.4874200230199));
#11604=CARTESIAN_POINT('Ctrl Pts',(0.0650184974572605,2.01060713514325,
24.4860303792198));
#11605=CARTESIAN_POINT('Ctrl Pts',(0.0997340039424784,2.01032309156194,
24.4846414817334));
#11606=CARTESIAN_POINT('Ctrl Pts',(0.134459334270958,2.00915694524383,24.4832528492418));
#11607=CARTESIAN_POINT('Ctrl Pts',(0.147933596547958,2.00870445246132,24.4827140264798));
#11608=CARTESIAN_POINT('Ctrl Pts',(0.161409337218446,2.00811912255674,24.482175243616));
#11609=CARTESIAN_POINT('Ctrl Pts',(0.174884610787376,2.00740143335556,24.4816364725311));
#11610=CARTESIAN_POINT('Ctrl Pts',(0.189332023983714,2.00663196827694,24.4810588331649));
#11611=CARTESIAN_POINT('Ctrl Pts',(0.203769295159425,2.00571085084408,24.4804815912802));
#11612=CARTESIAN_POINT('Ctrl Pts',(0.218191263309744,2.00463947026819,24.4799048229404));
#11613=CARTESIAN_POINT('Ctrl Pts',(0.293616304880072,1.99903628742713,24.4768883985829));
#11614=CARTESIAN_POINT('Ctrl Pts',(0.368646680368959,1.9893261617957,24.4738839495771));
#11615=CARTESIAN_POINT('Ctrl Pts',(0.44294146325047,1.97565502596793,24.4708866901775));
#11616=CARTESIAN_POINT('Ctrl Pts',(0.517780644499032,1.96188371427677,24.4678674682248));
#11617=CARTESIAN_POINT('Ctrl Pts',(0.591874413926822,1.94409297499423,24.4648555416287));
#11618=CARTESIAN_POINT('Ctrl Pts',(0.664872416764246,1.92237927515082,24.4618460186679));
#11619=CARTESIAN_POINT('Ctrl Pts',(0.693612873435508,1.91383025154381,24.4606611223571));
#11620=CARTESIAN_POINT('Ctrl Pts',(0.722183370632896,1.90467256243273,24.4594765986387));
#11621=CARTESIAN_POINT('Ctrl Pts',(0.750561917361623,1.89490995728419,24.4582921489677));
#11622=CARTESIAN_POINT('Ctrl Pts',(0.762696377885477,1.8907355382092,24.4577856868887));
#11623=CARTESIAN_POINT('Ctrl Pts',(0.774794416283802,1.88645088041849,24.4572792924806));
#11624=CARTESIAN_POINT('Ctrl Pts',(0.786842875051873,1.88206068413371,24.4567734253696));
#11625=CARTESIAN_POINT('Ctrl Pts',(0.859169502120084,1.85570643455227,24.4537367164772));
#11626=CARTESIAN_POINT('Ctrl Pts',(0.929822756867472,1.82551496441967,24.4507143015495));
#11627=CARTESIAN_POINT('Ctrl Pts',(0.998456357996127,1.79162107203564,24.4477013393046));
#11628=CARTESIAN_POINT('Ctrl Pts',(1.06668990494531,1.75792474167785,24.4447059391301));
#11629=CARTESIAN_POINT('Ctrl Pts',(1.13292826279404,1.7205687402294,24.4417198817631));
#11630=CARTESIAN_POINT('Ctrl Pts',(1.19681843662805,1.67963606311431,24.4387384100862));
#11631=CARTESIAN_POINT('Ctrl Pts',(1.24693212411197,1.64752960188985,24.4363998260615));
#11632=CARTESIAN_POINT('Ctrl Pts',(1.29560102816851,1.61322162205542,24.4340640633369));
#11633=CARTESIAN_POINT('Ctrl Pts',(1.34264328707622,1.57673230368136,24.4317288262356));
#11634=CARTESIAN_POINT('Ctrl Pts',(1.36662257672075,1.55813226289803,24.4305384640349));
#11635=CARTESIAN_POINT('Ctrl Pts',(1.39017901233764,1.53896516305314,24.429348238409));
#11636=CARTESIAN_POINT('Ctrl Pts',(1.41328706967152,1.51923201753369,24.4281578453009));
#11637=CARTESIAN_POINT('Ctrl Pts',(1.42306877589838,1.51087892105247,24.4276539485212));
#11638=CARTESIAN_POINT('Ctrl Pts',(1.4327701259467,1.50242438406759,24.427150021731));
#11639=CARTESIAN_POINT('Ctrl Pts',(1.44238912178932,1.49386842480447,24.4266460418679));
#11640=CARTESIAN_POINT('Ctrl Pts',(1.45230713194123,1.48504649658875,24.4261263953808));
#11641=CARTESIAN_POINT('Ctrl Pts',(1.46213208274873,1.47612156735597,24.4256069790412));
#11642=CARTESIAN_POINT('Ctrl Pts',(1.47185655624505,1.46709927890788,24.425088065848));
#11643=CARTESIAN_POINT('Ctrl Pts',(1.47412964601262,1.46499032446843,24.4249667702046));
#11644=CARTESIAN_POINT('Ctrl Pts',(1.47639734253898,1.4628759644146,24.4248454969878));
#11645=CARTESIAN_POINT('Ctrl Pts',(1.47865962347614,1.46075620613088,24.4247242458888));
#11646=CARTESIAN_POINT('Ctrl Pts',(1.53215475670349,1.41063124157184,24.4218570760403));
#11647=CARTESIAN_POINT('Ctrl Pts',(1.5826240221007,1.35749162418093,24.4190022736264));
#11648=CARTESIAN_POINT('Ctrl Pts',(1.6300398879693,1.30171088713118,24.4161557575599));
#11649=CARTESIAN_POINT('Ctrl Pts',(1.68078212606171,1.24201695581728,24.4131095494325));
#11650=CARTESIAN_POINT('Ctrl Pts',(1.72802829283498,1.17929792584938,24.4100728310601));
#11651=CARTESIAN_POINT('Ctrl Pts',(1.77170626798428,1.11396230694137,24.4070406007886));
#11652=CARTESIAN_POINT('Ctrl Pts',(1.80992449623993,1.05679364039686,24.404387399301));
#11653=CARTESIAN_POINT('Ctrl Pts',(1.84541040747536,0.997620449183277,24.4017376340156));
#11654=CARTESIAN_POINT('Ctrl Pts',(1.87808726172145,0.936693707274591,24.3990879542148));
#11655=CARTESIAN_POINT('Ctrl Pts',(1.88890052248433,0.916532135333474,24.3982111354608));
#11656=CARTESIAN_POINT('Ctrl Pts',(1.89940594781383,0.896178406839887,24.3973343260678));
#11657=CARTESIAN_POINT('Ctrl Pts',(1.90960005205868,0.875641268784333,24.3964574046166));
#11658=CARTESIAN_POINT('Ctrl Pts',(1.91547518951183,0.863805161749081,24.3959520111129));
#11659=CARTESIAN_POINT('Ctrl Pts',(1.92124762238796,0.851906634807171,24.3954465171147));
#11660=CARTESIAN_POINT('Ctrl Pts',(1.92691441011101,0.839952030543744,24.3949410974597));
#11661=CARTESIAN_POINT('Ctrl Pts',(1.96031903083694,0.769481943985819,24.3919617460688));
#11662=CARTESIAN_POINT('Ctrl Pts',(1.98992816786267,0.697337983571344,24.3889964420272));
#11663=CARTESIAN_POINT('Ctrl Pts',(2.0156863162126,0.623908778644958,24.3860406309664));
#11664=CARTESIAN_POINT('Ctrl Pts',(2.04178778214467,0.549500872270339,24.3830454233662));
#11665=CARTESIAN_POINT('Ctrl Pts',(2.06393536696727,0.473772310543712,24.3800599634878));
#11666=CARTESIAN_POINT('Ctrl Pts',(2.08202723354027,0.397097517940733,24.3770795124158));
#11667=CARTESIAN_POINT('Ctrl Pts',(2.09876155552511,0.326176109010256,24.3743227030122));
#11668=CARTESIAN_POINT('Ctrl Pts',(2.11202575380227,0.2544442193714,24.3715701789334));
#11669=CARTESIAN_POINT('Ctrl Pts',(2.12170133232151,0.182186358988051,24.3688181899904));
#11670=CARTESIAN_POINT('Ctrl Pts',(2.12533324744348,0.155062976620213,24.3677851778312));
#11671=CARTESIAN_POINT('Ctrl Pts',(2.12845912993511,0.127865424475548,24.3667522410737));
#11672=CARTESIAN_POINT('Ctrl Pts',(2.13107126614788,0.100608649754695,24.3657191813693));
#11673=CARTESIAN_POINT('Ctrl Pts',(2.1325759123382,0.0849081659730918,24.3651241169385));
#11674=CARTESIAN_POINT('Ctrl Pts',(2.13391008218326,0.0691880322062874,
24.3645290117138));
#11675=CARTESIAN_POINT('Ctrl Pts',(2.13507217604384,0.0534511129096754,
24.363933827786));
#11676=CARTESIAN_POINT('Ctrl Pts',(2.1358949975935,0.0423085737726864,24.363512407298));
#11677=CARTESIAN_POINT('Ctrl Pts',(2.13663134775102,0.0311597107005095,
24.3630910265538));
#11678=CARTESIAN_POINT('Ctrl Pts',(2.13728034324863,0.0200145848943864,
24.3626700130043));
#11679=CARTESIAN_POINT('Ctrl Pts',(2.14206066436502,-0.0620773254988428,
24.3595689437853));
#11680=CARTESIAN_POINT('Ctrl Pts',(2.14211688472276,-0.144103698334206,
24.3564825474227));
#11681=CARTESIAN_POINT('Ctrl Pts',(2.13733830774908,-0.22565130659055,24.3534056763928));
#11682=CARTESIAN_POINT('Ctrl Pts',(2.13255973077539,-0.307198914846895,
24.3503288053629));
#11683=CARTESIAN_POINT('Ctrl Pts',(2.1229467821906,-0.38826895977034,24.3472614596657));
#11684=CARTESIAN_POINT('Ctrl Pts',(2.10832870393275,-0.468456219886853,
24.3441984917776));
#11685=CARTESIAN_POINT('Ctrl Pts',(2.09441595298606,-0.544774417082047,
24.3412833131451));
#11686=CARTESIAN_POINT('Ctrl Pts',(2.07596888070456,-0.620293811415302,
24.3383721000521));
#11687=CARTESIAN_POINT('Ctrl Pts',(2.05323813750186,-0.694760696394361,
24.3354604147107));
#11688=CARTESIAN_POINT('Ctrl Pts',(2.04535336849461,-0.720591536218365,
24.3344504184191));
#11689=CARTESIAN_POINT('Ctrl Pts',(2.0369527279183,-0.746295609744288,24.3334403653049));
#11690=CARTESIAN_POINT('Ctrl Pts',(2.02804532218294,-0.771861842203744,
24.3324300701461));
#11691=CARTESIAN_POINT('Ctrl Pts',(2.02399375543204,-0.783490738479032,
24.3319705336217));
#11692=CARTESIAN_POINT('Ctrl Pts',(2.0198389575898,-0.795086319358417,24.3315111358951));
#11693=CARTESIAN_POINT('Ctrl Pts',(2.01558473198086,-0.806640549867355,
24.3310521410104));
#11694=CARTESIAN_POINT('Ctrl Pts',(1.98850593400829,-0.880184997774034,
24.3281305682272));
#11695=CARTESIAN_POINT('Ctrl Pts',(1.95737281308123,-0.952142606058721,
24.3252218392429));
#11696=CARTESIAN_POINT('Ctrl Pts',(1.92249757285567,-1.02227201743633,24.3223216485138));
#11697=CARTESIAN_POINT('Ctrl Pts',(1.88695067262014,-1.09375204664024,24.3193656031979));
#11698=CARTESIAN_POINT('Ctrl Pts',(1.84751568956125,-1.16333359394599,24.3164184281795));
#11699=CARTESIAN_POINT('Ctrl Pts',(1.80446912728237,-1.23074844857256,24.3134755643329));
#11700=CARTESIAN_POINT('Ctrl Pts',(1.76126023236668,-1.29841753095931,24.3105216026698));
#11701=CARTESIAN_POINT('Ctrl Pts',(1.71441188113122,-1.36390438374644,24.3075719847555));
#11702=CARTESIAN_POINT('Ctrl Pts',(1.66415769946571,-1.42691271211585,24.3046220996905));
#11703=CARTESIAN_POINT('Ctrl Pts',(1.64674427416882,-1.44874553841568,24.3035999438916));
#11704=CARTESIAN_POINT('Ctrl Pts',(1.62892155760558,-1.47028049720965,24.3025777560166));
#11705=CARTESIAN_POINT('Ctrl Pts',(1.61069818584296,-1.49150427719069,24.3015553442334));
#11706=CARTESIAN_POINT('Ctrl Pts',(1.60049069069606,-1.5033923972366,24.3009826585937));
#11707=CARTESIAN_POINT('Ctrl Pts',(1.59015563953053,-1.51518477143648,24.3004098063768));
#11708=CARTESIAN_POINT('Ctrl Pts',(1.57971072759172,-1.52686130763077,24.2998376300385));
#11709=CARTESIAN_POINT('Ctrl Pts',(1.5241196874745,-1.58900743158191,24.2967923312403));
#11710=CARTESIAN_POINT('Ctrl Pts',(1.46532985685416,-1.6479828288116,24.2937609986882));
#11711=CARTESIAN_POINT('Ctrl Pts',(1.40364751528756,-1.70349947958641,24.290738760932));
#11712=CARTESIAN_POINT('Ctrl Pts',(1.34352976106267,-1.75760793724063,24.2877931829591));
#11713=CARTESIAN_POINT('Ctrl Pts',(1.28066352510377,-1.80843159489564,24.2848562442503));
#11714=CARTESIAN_POINT('Ctrl Pts',(1.21529029695891,-1.85567350385066,24.2819234347283));
#11715=CARTESIAN_POINT('Ctrl Pts',(1.151018429448,-1.90211951545945,24.2790400350497));
#11716=CARTESIAN_POINT('Ctrl Pts',(1.08432265151975,-1.94510411645588,24.2761606265988));
#11717=CARTESIAN_POINT('Ctrl Pts',(1.01540230218933,-1.98430534234295,24.2732809234275));
#11718=CARTESIAN_POINT('Ctrl Pts',(0.991413070221145,-1.99795018469181,
24.2722785798809));
#11719=CARTESIAN_POINT('Ctrl Pts',(0.967154098038469,-2.01113625193634,
24.2712762006278));
#11720=CARTESIAN_POINT('Ctrl Pts',(0.942633141242275,-2.02384857830255,
24.2702736049284));
#11721=CARTESIAN_POINT('Ctrl Pts',(0.927689229189158,-2.03159590597765,
24.2696625887238));
#11722=CARTESIAN_POINT('Ctrl Pts',(0.91264425065672,-2.03916896131714,24.269051342741));
#11723=CARTESIAN_POINT('Ctrl Pts',(0.89752523548915,-2.04655226315939,24.2684408416994));
#11724=CARTESIAN_POINT('Ctrl Pts',(0.858076293954018,-2.06581697316084,
24.2668479059406));
#11725=CARTESIAN_POINT('Ctrl Pts',(0.818092741329694,-2.08380677668847,
24.2652587702448));
#11726=CARTESIAN_POINT('Ctrl Pts',(0.777614563358231,-2.10047761443662,
24.2636727376664));
#11727=CARTESIAN_POINT('Ctrl Pts',(0.705244379734806,-2.13028309604305,
24.2608370994365));
#11728=CARTESIAN_POINT('Ctrl Pts',(0.631294604316736,-2.15587544510049,
24.2580113803836));
#11729=CARTESIAN_POINT('Ctrl Pts',(0.556119155090156,-2.17737629254266,
24.2551915974639));
#11730=CARTESIAN_POINT('Ctrl Pts',(0.474948448561465,-2.20059183692319,
24.2521469362853));
#11731=CARTESIAN_POINT('Ctrl Pts',(0.392348029526542,-2.21903791275238,
24.24910919581));
#11732=CARTESIAN_POINT('Ctrl Pts',(0.308737702730448,-2.23280813351095,
24.2460733620308));
#11733=CARTESIAN_POINT('Ctrl Pts',(0.270500156739416,-2.23910567437389,
24.2446849828891));
#11734=CARTESIAN_POINT('Ctrl Pts',(0.232051123492098,-2.2444244113041,24.243297002535));
#11735=CARTESIAN_POINT('Ctrl Pts',(0.193429913054559,-2.24876906028139,
24.2419089413729));
#11736=CARTESIAN_POINT('Ctrl Pts',(0.161572159376237,-2.25235286191187,
24.2407639614488));
#11737=CARTESIAN_POINT('Ctrl Pts',(0.129597238881117,-2.25527382408218,
24.2396189265412));
#11738=CARTESIAN_POINT('Ctrl Pts',(0.0975271844407983,-2.25753324335174,
24.2384735674698));
#11739=CARTESIAN_POINT('Ctrl Pts',(0.0844330795511259,-2.25845575731131,
24.2380059208731));
#11740=CARTESIAN_POINT('Ctrl Pts',(0.0713229194369418,-2.25926790250605,
24.237538213561));
#11741=CARTESIAN_POINT('Ctrl Pts',(0.0582132985134477,-2.25996914699854,
24.2370709640795));
#11742=CARTESIAN_POINT('Ctrl Pts',(-0.023786791539092,-2.26435539980234,
24.2341483395591));
#11743=CARTESIAN_POINT('Ctrl Pts',(-0.105909169640656,-2.26441794064745,
24.231238450421));
#11744=CARTESIAN_POINT('Ctrl Pts',(-0.187776168973137,-2.26027172560533,
24.2283369940797));
#11745=CARTESIAN_POINT('Ctrl Pts',(-0.270727942589467,-2.25607057136317,
24.2253970921468));
#11746=CARTESIAN_POINT('Ctrl Pts',(-0.353418510685726,-2.24754840827001,
24.2224658479679));
#11747=CARTESIAN_POINT('Ctrl Pts',(-0.435464876948505,-2.23477219179204,
24.2195387856475));
#11748=CARTESIAN_POINT('Ctrl Pts',(-0.521020187243656,-2.22144956441731,
24.2164865392595));
#11749=CARTESIAN_POINT('Ctrl Pts',(-0.605876258185628,-2.20350155640051,
24.2134388400769));
#11750=CARTESIAN_POINT('Ctrl Pts',(-0.689592299481867,-2.18094418517737,
24.2103906130211));
#11751=CARTESIAN_POINT('Ctrl Pts',(-0.715540316679378,-2.17395246593974,
24.2094458066632));
#11752=CARTESIAN_POINT('Ctrl Pts',(-0.741378688380784,-2.16651748416069,
24.2085009495923));
#11753=CARTESIAN_POINT('Ctrl Pts',(-0.767093865522165,-2.15863854180591,
24.2075558906856));
#11754=CARTESIAN_POINT('Ctrl Pts',(-0.784576923837654,-2.15328186050072,
24.206913370516));
#11755=CARTESIAN_POINT('Ctrl Pts',(-0.802008196225349,-2.14771811367944,
24.2062705645783));
#11756=CARTESIAN_POINT('Ctrl Pts',(-0.819353040276014,-2.14195738810084,
24.2056285513437));
#11757=CARTESIAN_POINT('Ctrl Pts',(-0.899037670057529,-2.11549181229842,
24.2026790531084));
#11758=CARTESIAN_POINT('Ctrl Pts',(-0.977003896633911,-2.08484340063866,
24.1997424358208));
#11759=CARTESIAN_POINT('Ctrl Pts',(-1.05286862408811,-2.05008525245381,
24.1968142780767));
#11760=CARTESIAN_POINT('Ctrl Pts',(-1.12747088425221,-2.01590551569441,
24.1939348478968));
#11761=CARTESIAN_POINT('Ctrl Pts',(-1.20004195612714,-1.97775145483,24.1910635980521));
#11762=CARTESIAN_POINT('Ctrl Pts',(-1.27020612803878,-1.93564432789156,
24.1881963242159));
#11763=CARTESIAN_POINT('Ctrl Pts',(-1.31141969883518,-1.91091111990478,
24.1865121228633));
#11764=CARTESIAN_POINT('Ctrl Pts',(-1.35180254492918,-1.88481311495997,
24.1848292933302));
#11765=CARTESIAN_POINT('Ctrl Pts',(-1.3912746538158,-1.85734710164506,24.1831469835552));
#11766=CARTESIAN_POINT('Ctrl Pts',(-1.42843599657615,-1.83148899667307,
24.1815631591297));
#11767=CARTESIAN_POINT('Ctrl Pts',(-1.4647901026478,-1.80441827314899,24.1799797953884));
#11768=CARTESIAN_POINT('Ctrl Pts',(-1.50031387059669,-1.77619110968528,
24.1783961813238));
#11769=CARTESIAN_POINT('Ctrl Pts',(-1.52215895337135,-1.75883302077856,
24.1774223493707));
#11770=CARTESIAN_POINT('Ctrl Pts',(-1.54368997973301,-1.74103754278265,
24.1764484227568));
#11771=CARTESIAN_POINT('Ctrl Pts',(-1.56490095433692,-1.72281708855658,
24.1754742361418));
#11772=CARTESIAN_POINT('Ctrl Pts',(-1.57363676202097,-1.71531293624829,
24.1750730142708));
#11773=CARTESIAN_POINT('Ctrl Pts',(-1.58231716468627,-1.70773758138891,
24.1746717978913));
#11774=CARTESIAN_POINT('Ctrl Pts',(-1.59093464169824,-1.7000984316877,24.1742709109446));
#11775=CARTESIAN_POINT('Ctrl Pts',(-1.65233345722648,-1.6456701178499,24.1714146243938));
#11776=CARTESIAN_POINT('Ctrl Pts',(-1.71064235138754,-1.5879200224839,24.1685703732265));
#11777=CARTESIAN_POINT('Ctrl Pts',(-1.7657711224227,-1.52723905871173,24.1657341439519));
#11778=CARTESIAN_POINT('Ctrl Pts',(-1.82208471200389,-1.46525394957374,
24.1628369589008));
#11779=CARTESIAN_POINT('Ctrl Pts',(-1.87508056446529,-1.40020996058436,
24.1599481442582));
#11780=CARTESIAN_POINT('Ctrl Pts',(-1.9246306784322,-1.33247774123381,24.1570634221601));
#11781=CARTESIAN_POINT('Ctrl Pts',(-1.97456954733109,-1.26421411575282,
24.154156067421));
#11782=CARTESIAN_POINT('Ctrl Pts',(-2.02100893183075,-1.19321907898066,
24.1512528696959));
#11783=CARTESIAN_POINT('Ctrl Pts',(-2.0637776491882,-1.11983747840203,24.1483494496407));
#11784=CARTESIAN_POINT('Ctrl Pts',(-2.0795834502622,-1.09271824142458,24.1472764485627));
#11785=CARTESIAN_POINT('Ctrl Pts',(-2.09488748613988,-1.06527277805129,
24.1462034171193));
#11786=CARTESIAN_POINT('Ctrl Pts',(-2.10967951463669,-1.03751766643348,
24.1451301342659));
#11787=CARTESIAN_POINT('Ctrl Pts',(-2.11587483425371,-1.02589304121624,
24.1446806130716));
#11788=CARTESIAN_POINT('Ctrl Pts',(-2.12198032795743,-1.01421409411385,
24.1442310477757));
#11789=CARTESIAN_POINT('Ctrl Pts',(-2.12799519446604,-1.00248202627111,
24.1437814221381));
#11790=CARTESIAN_POINT('Ctrl Pts',(-2.13396603477409,-0.990835832050165,
24.1433350875641));
#11791=CARTESIAN_POINT('Ctrl Pts',(-2.13984317964154,-0.979145837240882,
24.1428890211268));
#11792=CARTESIAN_POINT('Ctrl Pts',(-2.14562556976068,-0.967414792131108,
24.142443258451));
#11793=CARTESIAN_POINT('Ctrl Pts',(-2.18361797146055,-0.890337568182734,
24.1395144358891));
#11794=CARTESIAN_POINT('Ctrl Pts',(-2.21753276717342,-0.811472272895308,
24.136598003258));
#11795=CARTESIAN_POINT('Ctrl Pts',(-2.24724034073236,-0.731200385356096,
24.133689629466));
#11796=CARTESIAN_POINT('Ctrl Pts',(-2.27690411613959,-0.651046843406481,
24.1307855435165));
#11797=CARTESIAN_POINT('Ctrl Pts',(-2.30237352692883,-0.56948993524845,
24.1278894926613));
#11798=CARTESIAN_POINT('Ctrl Pts',(-2.32347574001613,-0.486881735692151,
24.1249971649368));
#11799=CARTESIAN_POINT('Ctrl Pts',(-2.34386305936945,-0.407072109157236,
24.1222028225259));
#11800=CARTESIAN_POINT('Ctrl Pts',(-2.36017424532588,-0.326280337423849,
24.1194119552567));
#11801=CARTESIAN_POINT('Ctrl Pts',(-2.37220829744034,-0.244811300888254,
24.1166206747247));
#11802=CARTESIAN_POINT('Ctrl Pts',(-2.37735577292346,-0.209963531889701,
24.1154267254241));
#11803=CARTESIAN_POINT('Ctrl Pts',(-2.38172009802993,-0.174991762461182,
24.1142327005114));
#11804=CARTESIAN_POINT('Ctrl Pts',(-2.38528276313686,-0.139919699510735,
24.1130382956749));
#11805=CARTESIAN_POINT('Ctrl Pts',(-2.38690272774666,-0.123972227866057,
24.1124951928273));
#11806=CARTESIAN_POINT('Ctrl Pts',(-2.38835698230774,-0.10800180593106,
24.1119519365248));
#11807=CARTESIAN_POINT('Ctrl Pts',(-2.38964215962342,-0.0920336681917538,
24.1114092786465));
#11808=CARTESIAN_POINT('Ctrl Pts',(-2.39213828655412,-0.0610196608964784,
24.1103553050604));
#11809=CARTESIAN_POINT('Ctrl Pts',(-2.3939987663675,-0.0299955611709274,
24.1093029502777));
#11810=CARTESIAN_POINT('Ctrl Pts',(-2.39521656654617,0.001021571385391,
24.1082520127107));
#11811=CARTESIAN_POINT('',(0.159585929069883,2.44139648025874,24.0495));
#11812=CARTESIAN_POINT('Ctrl Pts',(0.159495341663529,2.44078487595686,24.0495));
#11813=CARTESIAN_POINT('Ctrl Pts',(0.074066622340348,2.43585402826852,24.0598924200211));
#11814=CARTESIAN_POINT('Ctrl Pts',(-0.010859609583587,2.42667871388636,
24.0703216585747));
#11815=CARTESIAN_POINT('Ctrl Pts',(-0.094920089983451,2.41327471514423,
24.080805508462));
#11816=CARTESIAN_POINT('Ctrl Pts',(-0.176987040604973,2.4001885978907,24.0910407294235));
#11817=CARTESIAN_POINT('Ctrl Pts',(-0.258229635425402,2.38307157874212,
24.1013280021715));
#11818=CARTESIAN_POINT('Ctrl Pts',(-0.338289104553414,2.36189432291947,
24.1116838833996));
#11819=CARTESIAN_POINT('Ctrl Pts',(-0.397114404548053,2.3463339096367,24.1192930747493));
#11820=CARTESIAN_POINT('Ctrl Pts',(-0.455300575655561,2.32858051294793,
24.126939306927));
#11821=CARTESIAN_POINT('Ctrl Pts',(-0.512694147882364,2.30860859110673,
24.1346291478542));
#11822=CARTESIAN_POINT('Ctrl Pts',(-0.555739327052466,2.29362964972583,
24.1403965285497));
#11823=CARTESIAN_POINT('Ctrl Pts',(-0.598338485322387,2.2774025434246,24.1461884391666));
#11824=CARTESIAN_POINT('Ctrl Pts',(-0.640422373698764,2.25991242064119,
24.152007650547));
#11825=CARTESIAN_POINT('Ctrl Pts',(-0.653200954142075,2.25460162476243,
24.1537746274973));
#11826=CARTESIAN_POINT('Ctrl Pts',(-0.665933630679759,2.2491736383325,24.1555443500471));
#11827=CARTESIAN_POINT('Ctrl Pts',(-0.678613238495502,2.24363023951219,
24.1573161763736));
#11828=CARTESIAN_POINT('Ctrl Pts',(-0.751691414929867,2.21168118533612,
24.1675279935516));
#11829=CARTESIAN_POINT('Ctrl Pts',(-0.822765594480603,2.17600952669347,
24.1777755768916));
#11830=CARTESIAN_POINT('Ctrl Pts',(-0.891516000215402,2.1365999170335,24.1880762105869));
#11831=CARTESIAN_POINT('Ctrl Pts',(-0.928691853481322,2.11528970292891,
24.1936461391234));
#11832=CARTESIAN_POINT('Ctrl Pts',(-0.965187750721331,2.09288581138188,
24.1992315793692));
#11833=CARTESIAN_POINT('Ctrl Pts',(-1.00094891382958,2.06938099984342,24.2048352641135));
#11834=CARTESIAN_POINT('Ctrl Pts',(-1.06863380541471,2.02489361513802,24.215441317201));
#11835=CARTESIAN_POINT('Ctrl Pts',(-1.13368940850762,1.97646369796482,24.2261127272925));
#11836=CARTESIAN_POINT('Ctrl Pts',(-1.19591823356727,1.92440867374989,24.236868023152));
#11837=CARTESIAN_POINT('Ctrl Pts',(-1.25694043864282,1.8733629990194,24.247414773295));
#11838=CARTESIAN_POINT('Ctrl Pts',(-1.31524464581085,1.8188304042027,24.2580421876465));
#11839=CARTESIAN_POINT('Ctrl Pts',(-1.37059918672337,1.76109384934245,24.2687677379139));
#11840=CARTESIAN_POINT('Ctrl Pts',(-1.37922787016168,1.75209385681257,24.2704396400999));
#11841=CARTESIAN_POINT('Ctrl Pts',(-1.38778631348174,1.74301434343772,24.2721142293588));
#11842=CARTESIAN_POINT('Ctrl Pts',(-1.39626855939247,1.73386174862397,24.2737905875937));
#11843=CARTESIAN_POINT('Ctrl Pts',(-1.44977170631647,1.6761302668667,24.2843644900577));
#11844=CARTESIAN_POINT('Ctrl Pts',(-1.50010267921852,1.61565151228324,24.2949800103224));
#11845=CARTESIAN_POINT('Ctrl Pts',(-1.54711077140567,1.55273985902926,24.3056567313238));
#11846=CARTESIAN_POINT('Ctrl Pts',(-1.59401007223834,1.48997380291934,24.3163087430701));
#11847=CARTESIAN_POINT('Ctrl Pts',(-1.63760217101603,1.42478505545467,24.3270216726058));
#11848=CARTESIAN_POINT('Ctrl Pts',(-1.67768937555964,1.35746710940028,24.3378149672182));
#11849=CARTESIAN_POINT('Ctrl Pts',(-1.71708448207235,1.2913113949966,24.3484219176335));
#11850=CARTESIAN_POINT('Ctrl Pts',(-1.75309481729665,1.22309842468162,24.3591064821044));
#11851=CARTESIAN_POINT('Ctrl Pts',(-1.78548310123427,1.15310335933718,24.3698871179472));
#11852=CARTESIAN_POINT('Ctrl Pts',(-1.79513059553039,1.13225393752258,24.3730983446674));
#11853=CARTESIAN_POINT('Ctrl Pts',(-1.80445637075224,1.11124642477179,24.376318095461));
#11854=CARTESIAN_POINT('Ctrl Pts',(-1.81345325565301,1.09008821973168,24.3795468581352));
#11855=CARTESIAN_POINT('Ctrl Pts',(-1.82117410078255,1.07193091015893,24.3823176812415));
#11856=CARTESIAN_POINT('Ctrl Pts',(-1.82865272688874,1.05366262327258,24.3850951411792));
#11857=CARTESIAN_POINT('Ctrl Pts',(-1.83588435026998,1.0352880996252,24.3878795462433));
#11858=CARTESIAN_POINT('Ctrl Pts',(-1.84027022210393,1.02414422480222,24.3895682464287));
#11859=CARTESIAN_POINT('Ctrl Pts',(-1.84456465303352,1.01296257609607,24.3912593019588));
#11860=CARTESIAN_POINT('Ctrl Pts',(-1.84876261773455,1.00175544207809,24.3929510965693));
#11861=CARTESIAN_POINT('Ctrl Pts',(-1.87498362800088,0.931754287454496,
24.4035182563739));
#11862=CARTESIAN_POINT('Ctrl Pts',(-1.89749241407045,0.860640587905358,
24.4141322445436));
#11863=CARTESIAN_POINT('Ctrl Pts',(-1.91611893315911,0.788676151971129,
24.4248130114787));
#11864=CARTESIAN_POINT('Ctrl Pts',(-1.93444514215941,0.717871978242132,
24.4353215754354));
#11865=CARTESIAN_POINT('Ctrl Pts',(-1.94901332439558,0.646243438436678,
24.4458947822059));
#11866=CARTESIAN_POINT('Ctrl Pts',(-1.95961190993143,0.57404300926657,24.4565516327006));
#11867=CARTESIAN_POINT('Ctrl Pts',(-1.96989411958387,0.503997818121701,
24.4668903680583));
#11868=CARTESIAN_POINT('Ctrl Pts',(-1.97644009504731,0.433413724452126,
24.4773078280141));
#11869=CARTESIAN_POINT('Ctrl Pts',(-1.97900996395521,0.362534966344129,
24.4878213621914));
#11870=CARTESIAN_POINT('Ctrl Pts',(-1.98042268495318,0.323571146212466,
24.4936009140003));
#11871=CARTESIAN_POINT('Ctrl Pts',(-1.98063301484526,0.284518578367179,
24.4994094991982));
#11872=CARTESIAN_POINT('Ctrl Pts',(-1.97959496748079,0.245420714742538,
24.50525));
#11873=CARTESIAN_POINT('',(-1.82664886469444,1.63001483842228,24.0495));
#11874=CARTESIAN_POINT('Origin',(0.,0.,24.0495));
#11875=CARTESIAN_POINT('Ctrl Pts',(-2.39521656654617,0.001021571385391,
24.1082520127107));
#11876=CARTESIAN_POINT('Ctrl Pts',(-2.39739631790017,0.0565394123832736,
24.1063709302271));
#11877=CARTESIAN_POINT('Ctrl Pts',(-2.39751759691081,0.112034830010131,
24.1044943877483));
#11878=CARTESIAN_POINT('Ctrl Pts',(-2.39553324020752,0.167412233368244,
24.1026212294439));
#11879=CARTESIAN_POINT('Ctrl Pts',(-2.39254564629891,0.250786957616897,
24.0998010528444));
#11880=CARTESIAN_POINT('Ctrl Pts',(-2.38478792175979,0.333894356888358,
24.0969885473228));
#11881=CARTESIAN_POINT('Ctrl Pts',(-2.37251451712036,0.416446035661837,
24.0941797683107));
#11882=CARTESIAN_POINT('Ctrl Pts',(-2.35999928411089,0.50062426701053,24.0913156466721));
#11883=CARTESIAN_POINT('Ctrl Pts',(-2.34278840534906,0.584225486929525,
24.0884553998398));
#11884=CARTESIAN_POINT('Ctrl Pts',(-2.32109729603087,0.666939404154293,
24.0855948454564));
#11885=CARTESIAN_POINT('Ctrl Pts',(-2.31259055669967,0.699377843450882,
24.084473003778));
#11886=CARTESIAN_POINT('Ctrl Pts',(-2.30339418836639,0.731679697293737,
24.0833511147976));
#11887=CARTESIAN_POINT('Ctrl Pts',(-2.29351910700337,0.763825629065356,
24.0822289262454));
#11888=CARTESIAN_POINT('Ctrl Pts',(-2.28936411833043,0.77735118672735,24.0817567599358));
#11889=CARTESIAN_POINT('Ctrl Pts',(-2.28508844313765,0.790850716500235,
24.0812844851308));
#11890=CARTESIAN_POINT('Ctrl Pts',(-2.28069445625563,0.804317800009188,
24.0808122566953));
#11891=CARTESIAN_POINT('Ctrl Pts',(-2.2540220454743,0.886065787206666,24.0779457322492));
#11892=CARTESIAN_POINT('Ctrl Pts',(-2.22309404362808,0.966317231109224,
24.0750914824426));
#11893=CARTESIAN_POINT('Ctrl Pts',(-2.18818569208204,1.04477343365878,24.0722454631076));
#11894=CARTESIAN_POINT('Ctrl Pts',(-2.15278423629671,1.12433788350052,24.0693592418114));
#11895=CARTESIAN_POINT('Ctrl Pts',(-2.11328881800044,1.20205688667092,24.0664814851511));
#11896=CARTESIAN_POINT('Ctrl Pts',(-2.06993298717036,1.27760977683417,24.0636079751466));
#11897=CARTESIAN_POINT('Ctrl Pts',(-2.02664727870796,1.35304047011081,24.0607391126676));
#11898=CARTESIAN_POINT('Ctrl Pts',(-1.97951314196675,1.42631291964495,24.0578744831188));
#11899=CARTESIAN_POINT('Ctrl Pts',(-1.92871671623399,1.49708592005729,24.0550098889532));
#11900=CARTESIAN_POINT('Ctrl Pts',(-1.89615495226116,1.54245316198097,24.0531736133146));
#11901=CARTESIAN_POINT('Ctrl Pts',(-1.86208739606077,1.58679286825759,24.0513373522154));
#11902=CARTESIAN_POINT('Ctrl Pts',(-1.82655445601515,1.63000783787766,24.0495));
#11903=CARTESIAN_POINT('',(-1.5,-1.83697019872103E-16,25.));
#11904=CARTESIAN_POINT('',(-2.,-2.44929359829471E-16,24.5));
#11905=CARTESIAN_POINT('Origin',(0.,0.,25.));
#11906=CARTESIAN_POINT('Ctrl Pts',(1.42545942445496,-1.99324250386964,-0.263127385183172));
#11907=CARTESIAN_POINT('Ctrl Pts',(2.08802763447242,-1.51940949184021,-0.22080398276521));
#11908=CARTESIAN_POINT('Ctrl Pts',(2.89213498951261,0.132635996242408,-0.136157177929286));
#11909=CARTESIAN_POINT('Ctrl Pts',(1.45520218380153,2.50608301571523,-0.00918697067539983));
#11910=CARTESIAN_POINT('Ctrl Pts',(-1.31405113801543,2.57978936419321,0.117783236578486));
#11911=CARTESIAN_POINT('Ctrl Pts',(-2.88067287706129,0.297396321818725,
0.244753443832372));
#11912=CARTESIAN_POINT('Ctrl Pts',(-1.81260958243465,-2.25895247596901,
0.371723651086258));
#11913=CARTESIAN_POINT('Ctrl Pts',(0.913666777514348,-2.74797773594403,
0.498693858340144));
#11914=CARTESIAN_POINT('Ctrl Pts',(2.80409801069081,-0.723890240901197,
0.62566406559403));
#11915=CARTESIAN_POINT('Ctrl Pts',(2.12960253907237,1.96263403532227,0.752634272847918));
#11916=CARTESIAN_POINT('Ctrl Pts',(-0.492916539459615,2.8537447239999,0.879604480101801));
#11917=CARTESIAN_POINT('Ctrl Pts',(-2.66453975376405,1.13454357669983,1.00657468735569));
#11918=CARTESIAN_POINT('Ctrl Pts',(-2.39885204218408,-1.62249170425571,
1.13354489460957));
#11919=CARTESIAN_POINT('Ctrl Pts',(0.061126426924356,-2.89537413517611,
1.26051510186346));
#11920=CARTESIAN_POINT('Ctrl Pts',(2.46518916271889,-1.51979997447114,1.38748530911735));
#11921=CARTESIAN_POINT('Ctrl Pts',(2.61428569985594,1.24597721053458,1.51445551637123));
#11922=CARTESIAN_POINT('Ctrl Pts',(0.372032336604703,2.8720263299409,1.64142572362512));
#11923=CARTESIAN_POINT('Ctrl Pts',(-2.21052758161165,1.870966192965,1.76839593087901));
#11924=CARTESIAN_POINT('Ctrl Pts',(-2.77106544293345,-0.841512102466542,
1.89536613813289));
#11925=CARTESIAN_POINT('Ctrl Pts',(-0.796843696806246,-2.7842388029683,
2.02233634538678));
#11926=CARTESIAN_POINT('Ctrl Pts',(1.90626990835674,-2.1801562189121,2.14930655264067));
#11927=CARTESIAN_POINT('Ctrl Pts',(2.8656730678851,0.418167282282024,2.27627675989455));
#11928=CARTESIAN_POINT('Ctrl Pts',(1.20377683918878,2.63398315136886,2.40324696714844));
#11929=CARTESIAN_POINT('Ctrl Pts',(-1.5592427162438,2.4404319593272,2.53021717440232));
#11930=CARTESIAN_POINT('Ctrl Pts',(-2.89598584198633,0.0145595381614903,
2.65718738165621));
#11931=CARTESIAN_POINT('Ctrl Pts',(-1.58370177295115,-2.42463082992762,
2.7841575889101));
#11932=CARTESIAN_POINT('Ctrl Pts',(1.17723200946275,-2.64595366058855,2.91112779616398));
#11933=CARTESIAN_POINT('Ctrl Pts',(2.86132364740886,-0.446959684274638,
3.03809800341787));
#11934=CARTESIAN_POINT('Ctrl Pts',(1.92809442652916,2.16087895448481,3.16506821067175));
#11935=CARTESIAN_POINT('Ctrl Pts',(-0.768808667492088,2.79211017115979,
3.29203841792564));
#11936=CARTESIAN_POINT('Ctrl Pts',(-2.76246417072418,0.869331743334865,
3.41900862517952));
#11937=CARTESIAN_POINT('Ctrl Pts',(-2.22922793215949,-1.84864512573327,
3.54597883243341));
#11938=CARTESIAN_POINT('Ctrl Pts',(0.343136166208384,-2.87562228849207,
3.67294903968729));
#11939=CARTESIAN_POINT('Ctrl Pts',(2.60162544445905,-1.27219928520545,3.79991924694119));
#11940=CARTESIAN_POINT('Ctrl Pts',(2.4803459928753,1.49493469093412,3.92688945419507));
#11941=CARTESIAN_POINT('Ctrl Pts',(0.0902350130762593,2.89461631602099,
4.05385966144895));
#11942=CARTESIAN_POINT('Ctrl Pts',(-2.38241608137131,1.64652348594472,4.18082986870284));
#11943=CARTESIAN_POINT('Ctrl Pts',(-2.67581446902845,-1.10768357480063,
4.30780007595673));
#11944=CARTESIAN_POINT('Ctrl Pts',(-0.521581659896502,-2.84866609952948,
4.43477028321062));
#11945=CARTESIAN_POINT('Ctrl Pts',(2.10975431061419,-1.98390592604371,4.5617404904645));
#11946=CARTESIAN_POINT('Ctrl Pts',(2.8112477871886,0.695580227992425,4.68871069771839));
#11947=CARTESIAN_POINT('Ctrl Pts',(0.941225986649517,2.73880258810359,4.81568090497227));
#11948=CARTESIAN_POINT('Ctrl Pts',(-1.78975763124189,2.27677701937592,4.94265111222616));
#11949=CARTESIAN_POINT('Ctrl Pts',(-2.88360733584287,-0.267870691230269,
5.06962131948004));
#11950=CARTESIAN_POINT('Ctrl Pts',(-1.33975276154346,-2.56749070348536,
5.19659152673394));
#11951=CARTESIAN_POINT('Ctrl Pts',(1.42960555866,-2.51856584611072,5.32356173398781));
#11952=CARTESIAN_POINT('Ctrl Pts',(2.89126964034985,-0.165848850880107,
5.4505319412417));
#11953=CARTESIAN_POINT('Ctrl Pts',(1.70822055079356,2.33857403654312,5.57750214849559));
#11954=CARTESIAN_POINT('Ctrl Pts',(-1.03737854344871,2.70384757930976,5.70447235574947));
#11955=CARTESIAN_POINT('Ctrl Pts',(-2.83406278757172,0.595847371940374,
5.83144256300336));
#11956=CARTESIAN_POINT('Ctrl Pts',(-2.03836233058378,-2.05718861162609,
5.95841277025725));
#11957=CARTESIAN_POINT('Ctrl Pts',(0.621876676608205,-2.82846519752988,
6.08538297751113));
#11958=CARTESIAN_POINT('Ctrl Pts',(2.71327028295494,-1.01247733119344,6.21235318476502));
#11959=CARTESIAN_POINT('Ctrl Pts',(2.32277096781915,1.72964765359987,6.33932339201891));
#11960=CARTESIAN_POINT('Ctrl Pts',(-0.192422248794526,2.88962275266442,
6.46629359927278));
#11961=CARTESIAN_POINT('Ctrl Pts',(-2.53160225352177,1.40639112785544,6.59326380652668));
#11962=CARTESIAN_POINT('Ctrl Pts',(-2.55506540818197,-1.3632999429542,6.72023401378057));
#11963=CARTESIAN_POINT('Ctrl Pts',(-0.241349406630154,-2.88594810044572,
6.84720422103445));
#11964=CARTESIAN_POINT('Ctrl Pts',(2.29313464286823,-1.76875082592903,6.97417442828833));
#11965=CARTESIAN_POINT('Ctrl Pts',(2.73003384286064,0.966364936958393,7.10114463554223));
#11966=CARTESIAN_POINT('Ctrl Pts',(0.669706094041877,2.81752368617376,7.2281148427961));
#11967=CARTESIAN_POINT('Ctrl Pts',(-2.00321776240315,2.09142644406622,7.35508505005));
#11968=CARTESIAN_POINT('Ctrl Pts',(-2.84375064183066,-0.547748356122364,
7.48205525730387));
#11969=CARTESIAN_POINT('Ctrl Pts',(-1.08303710922197,-2.6858846949553,7.60902546455777));
#11970=CARTESIAN_POINT('Ctrl Pts',(1.66835625059269,-2.36717836160593,7.73599567181165));
#11971=CARTESIAN_POINT('Ctrl Pts',(2.89366443014745,0.1168423735059,7.86296587906554));
#11972=CARTESIAN_POINT('Ctrl Pts',(1.47206886721645,2.49398460795553,7.98993608631941));
#11973=CARTESIAN_POINT('Ctrl Pts',(-1.29606313347053,2.58981974828473,8.11690629357332));
#11974=CARTESIAN_POINT('Ctrl Pts',(-2.87865533115204,0.316685110128232,
8.24387650082718));
#11975=CARTESIAN_POINT('Ctrl Pts',(-1.8280729665141,-2.24612893744935,8.37084670808109));
#11976=CARTESIAN_POINT('Ctrl Pts',(0.894691260744527,-2.75435537331231,
8.49781691533496));
#11977=CARTESIAN_POINT('Ctrl Pts',(2.79906009226845,-0.743107377447683,
8.62478712258886));
#11978=CARTESIAN_POINT('Ctrl Pts',(2.1430620213695,1.94787862740744,8.75175732984274));
#11979=CARTESIAN_POINT('Ctrl Pts',(-0.473245899435898,2.85709367946067,
8.87872753709663));
#11980=CARTESIAN_POINT('Ctrl Pts',(-2.65666452966483,1.15285712530556,9.0056977443505));
#11981=CARTESIAN_POINT('Ctrl Pts',(-2.4099688685346,-1.60592528694242,9.13266795160441));
#11982=CARTESIAN_POINT('Ctrl Pts',(0.0411826897410067,-2.8957296076486,
9.25963815885827));
#11983=CARTESIAN_POINT('Ctrl Pts',(2.45466346129185,-1.53674111884394,9.38660836611218));
#11984=CARTESIAN_POINT('Ctrl Pts',(2.62280512767723,1.22794105590498,9.51357857336605));
#11985=CARTESIAN_POINT('Ctrl Pts',(0.391804503777794,2.86939631375076,9.64054878061995));
#11986=CARTESIAN_POINT('Ctrl Pts',(-2.19758902724922,1.8861464529195,9.76751898787382));
#11987=CARTESIAN_POINT('Ctrl Pts',(-2.77679555799053,-0.822406471078079,
9.89448919512773));
#11988=CARTESIAN_POINT('Ctrl Pts',(-0.816001085855212,-2.77868461730189,
10.0214594023816));
#11989=CARTESIAN_POINT('Ctrl Pts',(1.89120900570025,-2.19323379312495,10.1484296096355));
#11990=CARTESIAN_POINT('Ctrl Pts',(2.86848519653882,0.398420195001009,10.2753998168894));
#11991=CARTESIAN_POINT('Ctrl Pts',(1.22188968930472,2.6256297457406,10.4023700241433));
#11992=CARTESIAN_POINT('Ctrl Pts',(-1.54239740574098,2.45111326080835,10.5293402313971));
#11993=CARTESIAN_POINT('Ctrl Pts',(-2.89581687456089,0.0345051236109951,
10.656310438651));
#11994=CARTESIAN_POINT('Ctrl Pts',(-1.60036370874777,-2.41366567160204,
10.7832806459049));
#11995=CARTESIAN_POINT('Ctrl Pts',(1.1589802406304,-2.6539990158957,10.9102508531588));
#11996=CARTESIAN_POINT('Ctrl Pts',(2.85817737255768,-0.466656277731571,
11.0372210604127));
#11997=CARTESIAN_POINT('Ctrl Pts',(1.94293161840177,2.14754806715978,11.1641912676666));
#11998=CARTESIAN_POINT('Ctrl Pts',(-0.749559941647221,2.79733906926294,
11.2911614749205));
#11999=CARTESIAN_POINT('Ctrl Pts',(-2.75641117861896,0.888337429658026,
11.4181316821743));
#12000=CARTESIAN_POINT('Ctrl Pts',(-2.24190748980745,-1.83324760512384,
11.5451018894282));
#12001=CARTESIAN_POINT('Ctrl Pts',(0.323322352062451,-2.87791741215828,
11.6720720966821));
#12002=CARTESIAN_POINT('Ctrl Pts',(2.59280154130405,-1.29008764894419,11.799042303936));
#12003=CARTESIAN_POINT('Ctrl Pts',(2.49058343499892,1.47781599932333,11.9260125111899));
#12004=CARTESIAN_POINT('Ctrl Pts',(0.11016936844703,2.89392617127718,12.0529827184438));
#12005=CARTESIAN_POINT('Ctrl Pts',(-2.37101924217833,1.66289317990276,12.1799529256976));
#12006=CARTESIAN_POINT('Ctrl Pts',(-2.68338010614347,-1.08922779091451,
12.3069231329516));
#12007=CARTESIAN_POINT('Ctrl Pts',(-0.541189304938158,-2.84500617060272,
12.4338933402054));
#12008=CARTESIAN_POINT('Ctrl Pts',(2.09604023735608,-1.99838967619712,12.5608635474593));
#12009=CARTESIAN_POINT('Ctrl Pts',(2.81597187500845,0.676201429833178,12.6878337547132));
#12010=CARTESIAN_POINT('Ctrl Pts',(0.960066999954102,2.73225498995722,12.8148039619671));
#12011=CARTESIAN_POINT('Ctrl Pts',(-1.77403401586218,2.28904986514295,12.941774169221));
#12012=CARTESIAN_POINT('Ctrl Pts',(-2.88538388370124,-0.248003665747437,
13.0687443764749));
#12013=CARTESIAN_POINT('Ctrl Pts',(-1.35740442202033,-2.55820233946158,
13.1957145837288));
#12014=CARTESIAN_POINT('Ctrl Pts',(1.41222517962834,-2.52835243124267,13.3226847909826));
#12015=CARTESIAN_POINT('Ctrl Pts',(2.89005878923091,-0.185758362762534,
13.4496549982365));
#12016=CARTESIAN_POINT('Ctrl Pts',(1.72428682193203,2.32675330240628,13.5766252054904));
#12017=CARTESIAN_POINT('Ctrl Pts',(-1.01873135074601,2.71092832984464,13.7035954127443));
#12018=CARTESIAN_POINT('Ctrl Pts',(-2.82989170439569,0.615352676064313,
13.8305656199982));
#12019=CARTESIAN_POINT('Ctrl Pts',(-2.05248274601473,-2.04310071994967,
13.9575358272521));
#12020=CARTESIAN_POINT('Ctrl Pts',(0.602381042723655,-2.83268124820181,
14.0845060345059));
#12021=CARTESIAN_POINT('Ctrl Pts',(2.7062325510552,-1.03114080229438,14.2114762417598));
#12022=CARTESIAN_POINT('Ctrl Pts',(2.33462871881716,1.71360868339922,14.3384464490137));
#12023=CARTESIAN_POINT('Ctrl Pts',(-0.172515582029027,2.89087951123947,
14.4654166562676));
#12024=CARTESIAN_POINT('Ctrl Pts',(-2.52185577298868,1.42379402821851,14.5923868635215));
#12025=CARTESIAN_POINT('Ctrl Pts',(-2.5643944516552,-1.34566974806862,14.7193570707754));
#12026=CARTESIAN_POINT('Ctrl Pts',(-0.261220475952221,-2.88421737001396,
14.8463272780293));
#12027=CARTESIAN_POINT('Ctrl Pts',(2.28089808786825,-1.78450270027982,14.9732974852832));
#12028=CARTESIAN_POINT('Ctrl Pts',(2.73662487035168,0.947539072291846,15.100267692537));
#12029=CARTESIAN_POINT('Ctrl Pts',(0.689095734268094,2.81284429778126,15.2272378997909));
#12030=CARTESIAN_POINT('Ctrl Pts',(-1.98876567495755,2.10517387991056,15.3542081070448));
#12031=CARTESIAN_POINT('Ctrl Pts',(-2.84745577560679,-0.528149202887348,
15.4811783142987));
#12032=CARTESIAN_POINT('Ctrl Pts',(-1.10151029014829,-2.6783616363823,15.6081485215526));
#12033=CARTESIAN_POINT('Ctrl Pts',(1.65201288089262,-2.3786129184699,15.7351187288065));
#12034=CARTESIAN_POINT('Ctrl Pts',(2.89440054101786,0.096909662586019,15.8620889360604));
#12035=CARTESIAN_POINT('Ctrl Pts',(1.48921112051991,2.48378666818768,15.9890591433142));
#12036=CARTESIAN_POINT('Ctrl Pts',(-1.27819516492898,2.59868487795254,16.1160293505682));
#12037=CARTESIAN_POINT('Ctrl Pts',(-2.87640590357244,0.33650416407621,16.242999557822));
#12038=CARTESIAN_POINT('Ctrl Pts',(-1.84349968485467,-2.23348491969114,
16.3699697650759));
#12039=CARTESIAN_POINT('Ctrl Pts',(0.875699583007191,-2.76045217579802,
16.4969399723298));
#12040=CARTESIAN_POINT('Ctrl Pts',(2.79387559488741,-0.762368109799676,
16.6239101795837));
#12041=CARTESIAN_POINT('Ctrl Pts',(2.15642708752431,1.93307221560355,16.7508803868376));
#12042=CARTESIAN_POINT('Ctrl Pts',(-0.453556613933447,2.86028536557181,
16.8778505940914));
#12043=CARTESIAN_POINT('Ctrl Pts',(-2.64866128299822,1.17112739806275,17.0048208013453));
#12044=CARTESIAN_POINT('Ctrl Pts',(-2.42097242095965,-1.58928868098272,
17.1317910085992));
#12045=CARTESIAN_POINT('Ctrl Pts',(0.0212375495843619,-2.8959445680183,
17.2587612158531));
#12046=CARTESIAN_POINT('Ctrl Pts',(2.4440210279303,-1.5536110161754,17.385731423107));
#12047=CARTESIAN_POINT('Ctrl Pts',(2.63120028826644,1.20984751831527,17.5127016303609));
#12048=CARTESIAN_POINT('Ctrl Pts',(0.411558005066825,2.8666297254812,17.6396718376148));
#12049=CARTESIAN_POINT('Ctrl Pts',(-2.1845461831526,1.90123747812324,17.7666420448687));
#12050=CARTESIAN_POINT('Ctrl Pts',(-2.78239397108689,-0.803261952420473,
17.8936122521225));
#12051=CARTESIAN_POINT('Ctrl Pts',(-0.835119754406293,-2.77299855217189,
18.0205824593764));
#12052=CARTESIAN_POINT('Ctrl Pts',(1.87605838296808,-2.20620736066268,18.1475526666303));
#12053=CARTESIAN_POINT('Ctrl Pts',(2.87116125492305,0.37865422587848,18.2745228738842));
#12054=CARTESIAN_POINT('Ctrl Pts',(1.23994457449353,2.61715177754961,18.4014930811381));
#12055=CARTESIAN_POINT('Ctrl Pts',(-1.52547892705471,2.46167829288456,18.528463288392));
#12056=CARTESIAN_POINT('Ctrl Pts',(-2.89551053760248,0.0544490695970991,
18.6554334956458));
#12057=CARTESIAN_POINT('Ctrl Pts',(-1.61694972722591,-2.40258601389651,
18.7824037028998));
#12058=CARTESIAN_POINT('Ctrl Pts',(1.14067349267392,-2.66191847314265,18.9093739101536));
#12059=CARTESIAN_POINT('Ctrl Pts',(2.85489551329953,-0.486330733852118,
19.0363441174075));
#12060=CARTESIAN_POINT('Ctrl Pts',(1.95767664263525,2.13411530556051,19.1633143246614));
#12061=CARTESIAN_POINT('Ctrl Pts',(-0.730275658617059,2.8024352690077,19.2902845319153));
#12062=CARTESIAN_POINT('Ctrl Pts',(-2.75022742957226,0.907300975517427,
19.4172547391691));
#12063=CARTESIAN_POINT('Ctrl Pts',(-2.25448069721154,-1.81776312000476,
19.5442249464231));
#12064=CARTESIAN_POINT('Ctrl Pts',(0.303493200345932,-2.88007601494976,
19.6711951536769));
#12065=CARTESIAN_POINT('Ctrl Pts',(2.58385464241264,-1.30791481428527,19.7981653609309));
#12066=CARTESIAN_POINT('Ctrl Pts',(2.5007027303468,1.4606272039764,19.9251355681847));
#12067=CARTESIAN_POINT('Ctrl Pts',(0.130098497667631,2.89309874622963,20.0521057754386));
#12068=CARTESIAN_POINT('Ctrl Pts',(-2.35950992801564,1.67918399055304,20.1790759826925));
#12069=CARTESIAN_POINT('Ctrl Pts',(-2.6908184507229,-1.07072033691426,20.3060461899464));
#12070=CARTESIAN_POINT('Ctrl Pts',(-0.560771277348947,-2.84121128199187,
20.4330163972002));
#12071=CARTESIAN_POINT('Ctrl Pts',(2.08222673337684,-2.01277862799546,20.5599866044542));
#12072=CARTESIAN_POINT('Ctrl Pts',(2.82056238055676,0.656790554509431,20.686956811708));
#12073=CARTESIAN_POINT('Ctrl Pts',(0.978862470027363,2.72557778064029,20.813927018962));
#12074=CARTESIAN_POINT('Ctrl Pts',(-1.75822624463689,2.30121412459989,20.9408972262158));
#12075=CARTESIAN_POINT('Ctrl Pts',(-2.88702355705684,-0.228124876075658,
21.0678674334697));
#12076=CARTESIAN_POINT('Ctrl Pts',(-1.37499168967642,-2.54879262012524,
21.1948376407236));
#12077=CARTESIAN_POINT('Ctrl Pts',(1.39477780622873,-2.53801907959506,21.3218078479775));
#12078=CARTESIAN_POINT('Ctrl Pts',(2.88871084525135,-0.20565905959194,21.4487780552314));
#12079=CARTESIAN_POINT('Ctrl Pts',(1.74027128981661,2.31482218714578,21.5757482624852));
#12080=CARTESIAN_POINT('Ctrl Pts',(-1.00003581763517,2.71788049248305,21.7027184697391));
#12081=CARTESIAN_POINT('Ctrl Pts',(-2.82558640606945,0.634828767624046,
21.829688676993));
#12082=CARTESIAN_POINT('Ctrl Pts',(-2.06650574459841,-2.02891586731337,
21.9566588842469));
#12083=CARTESIAN_POINT('Ctrl Pts',(0.582856733610425,-2.83676300309042,
22.0836290915008));
#12084=CARTESIAN_POINT('Ctrl Pts',(2.69906663270847,-1.04975520788588,22.2105992987547));
#12085=CARTESIAN_POINT('Ctrl Pts',(2.34637535894793,1.69748813671122,22.3375695060086));
#12086=CARTESIAN_POINT('Ctrl Pts',(-0.152600041786191,2.89199968134328,
22.4645397132624));
#12087=CARTESIAN_POINT('Ctrl Pts',(-2.5119909759523,1.44112834512521,22.5915099205164));
#12088=CARTESIAN_POINT('Ctrl Pts',(-2.57359934481574,-1.32797373282733,
22.7184801277702));
#12089=CARTESIAN_POINT('Ctrl Pts',(-0.281083919150256,-2.88235360097688,
22.8454503350241));
#12090=CARTESIAN_POINT('Ctrl Pts',(2.26856240924181,-1.80016272103242,22.972420542278));
#12091=CARTESIAN_POINT('Ctrl Pts',(2.74306879317415,0.928654543166714,23.0993907495319));
#12092=CARTESIAN_POINT('Ctrl Pts',(0.708485608711905,2.80805759792725,23.2263609567858));
#12093=CARTESIAN_POINT('Ctrl Pts',(-1.97428195070499,2.11877169925234,23.3533311640396));
#12094=CARTESIAN_POINT('Ctrl Pts',(-2.85090640203137,-0.508430235562458,
23.4803013712935));
#12095=CARTESIAN_POINT('Ctrl Pts',(-1.12015872947254,-2.6708920247376,23.6072715785474));
#12096=CARTESIAN_POINT('Ctrl Pts',(1.63602484856987,-2.38959065359107,23.7342417858013));
#12097=CARTESIAN_POINT('Ctrl Pts',(2.8941699184606,0.0763153981960129,23.8612119930552));
#12098=CARTESIAN_POINT('Ctrl Pts',(1.50789198472586,2.47473781233419,23.988182200309));
#12099=CARTESIAN_POINT('Ctrl Pts',(-1.26358600876801,2.60487763695496,24.115152407563));
#12100=CARTESIAN_POINT('Ctrl Pts',(-2.33166392375486,1.10986843944438,24.1997992123989));
#12101=CARTESIAN_POINT('Ctrl Pts',(-2.43188242527222,0.301493150257353,
24.2421226148168));
#12102=CARTESIAN_POINT('Ctrl Pts',(1.33708927785964,-1.86967312739702,-0.175418256788781));
#12103=CARTESIAN_POINT('Ctrl Pts',(1.9585821343145,-1.42521499059475,-0.133094854370819));
#12104=CARTESIAN_POINT('Ctrl Pts',(2.71283953668389,0.124413340282714,-0.0484480495348954));
#12105=CARTESIAN_POINT('Ctrl Pts',(1.36498816009652,2.3507205271874,0.0785221577189909));
#12106=CARTESIAN_POINT('Ctrl Pts',(-1.23258765353597,2.419857513179,0.205492364972877));
#12107=CARTESIAN_POINT('Ctrl Pts',(-2.70208800816096,0.278959489380628,
0.332462572226763));
#12108=CARTESIAN_POINT('Ctrl Pts',(-1.70023839054259,-2.11891063540273,
0.459432779480649));
#12109=CARTESIAN_POINT('Ctrl Pts',(0.857024781479203,-2.57761918963968,
0.586402986734535));
#12110=CARTESIAN_POINT('Ctrl Pts',(2.63026033560785,-0.679013280105372,
0.713373193988421));
#12111=CARTESIAN_POINT('Ctrl Pts',(1.997579638007,1.84096220486614,0.840343401242307));
#12112=CARTESIAN_POINT('Ctrl Pts',(-0.462358597154108,2.67682924308268,
0.967313608496194));
#12113=CARTESIAN_POINT('Ctrl Pts',(-2.49935387431386,1.06420851105598,1.09428381575008));
#12114=CARTESIAN_POINT('Ctrl Pts',(-2.25013724680555,-1.5219067087834,1.22125402300397));
#12115=CARTESIAN_POINT('Ctrl Pts',(0.0573369459924396,-2.71587787426249,
1.34822423025785));
#12116=CARTESIAN_POINT('Ctrl Pts',(2.3123618538827,-1.42558126558655,1.47519443751174));
#12117=CARTESIAN_POINT('Ctrl Pts',(2.45221527780476,1.16873391138456,1.60216464476562));
#12118=CARTESIAN_POINT('Ctrl Pts',(0.348968507806855,2.69397749638712,1.72913485201951));
#12119=CARTESIAN_POINT('Ctrl Pts',(-2.07348780125123,1.75497723255643,1.85610505927339));
#12120=CARTESIAN_POINT('Ctrl Pts',(-2.59927559383913,-0.789343274241099,
1.98307526652729));
#12121=CARTESIAN_POINT('Ctrl Pts',(-0.747444048459754,-2.61163228260472,
2.11004547378116));
#12122=CARTESIAN_POINT('Ctrl Pts',(1.78809232409043,-2.04499928539254,2.23701568103506));
#12123=CARTESIAN_POINT('Ctrl Pts',(2.68801809941763,0.392243356702178,2.36398588828894));
#12124=CARTESIAN_POINT('Ctrl Pts',(1.1291497162261,2.47069160253713,2.49095609554283));
#12125=CARTESIAN_POINT('Ctrl Pts',(-1.46257878807563,2.28913945229282,2.61792630279671));
#12126=CARTESIAN_POINT('Ctrl Pts',(-2.71645165882843,0.0136569319563776,
2.7448965100506));
#12127=CARTESIAN_POINT('Ctrl Pts',(-1.48552152633178,-2.27431790049286,
2.87186671730448));
#12128=CARTESIAN_POINT('Ctrl Pts',(1.10425051067844,-2.48192001020248,2.99883692455838));
#12129=CARTESIAN_POINT('Ctrl Pts',(2.68393831757051,-0.419250798182282,
3.12580713181225));
#12130=CARTESIAN_POINT('Ctrl Pts',(1.80856384979101,2.02691709860416,3.25277733906614));
#12131=CARTESIAN_POINT('Ctrl Pts',(-0.721147026982028,2.61901567200914,
3.37974754632003));
#12132=CARTESIAN_POINT('Ctrl Pts',(-2.59120755019672,0.815438260096795,
3.50671775357391));
#12133=CARTESIAN_POINT('Ctrl Pts',(-2.09102883944623,-1.73403994093382,
3.6336879608278));
#12134=CARTESIAN_POINT('Ctrl Pts',(0.321863730957119,-2.69735052654142,
3.76065816808169));
#12135=CARTESIAN_POINT('Ctrl Pts',(2.44033988419076,-1.19333037080265,3.88762837533557));
#12136=CARTESIAN_POINT('Ctrl Pts',(2.32657904922396,1.40225748418809,4.01459858258946));
#12137=CARTESIAN_POINT('Ctrl Pts',(0.084640970063364,2.71516703546239,4.14156878984334));
#12138=CARTESIAN_POINT('Ctrl Pts',(-2.23472021942679,1.54444866057315,4.26853899709723));
#12139=CARTESIAN_POINT('Ctrl Pts',(-2.50992962317935,-1.03901367216639,
4.39550920435112));
#12140=CARTESIAN_POINT('Ctrl Pts',(-0.489246647790451,-2.6720654636238,
4.522479411605));
#12141=CARTESIAN_POINT('Ctrl Pts',(1.97896188361798,-1.86091536278529,4.64944961885889));
#12142=CARTESIAN_POINT('Ctrl Pts',(2.63696686778288,0.652458322407474,4.77641982611277));
#12143=CARTESIAN_POINT('Ctrl Pts',(0.882875480845896,2.56901284729855,4.90339003336666));
#12144=CARTESIAN_POINT('Ctrl Pts',(-1.67880312665934,2.13563016137682,5.03036024062055));
#12145=CARTESIAN_POINT('Ctrl Pts',(-2.70484054766217,-0.251264275188861,
5.15733044787444));
#12146=CARTESIAN_POINT('Ctrl Pts',(-1.25669592673788,-2.40832129749834,
5.28430065512832));
#12147=CARTESIAN_POINT('Ctrl Pts',(1.34097837599531,-2.36242949511231,5.41127086238221));
#12148=CARTESIAN_POINT('Ctrl Pts',(2.71202783410766,-0.155567192199782,
5.5382410696361));
#12149=CARTESIAN_POINT('Ctrl Pts',(1.60232086827652,2.19359612493941,5.66521127688997));
#12150=CARTESIAN_POINT('Ctrl Pts',(-0.97306714153387,2.53622484459299,5.79218148414387));
#12151=CARTESIAN_POINT('Ctrl Pts',(-2.65836747159051,0.558908320078628,
5.91915169139774));
#12152=CARTESIAN_POINT('Ctrl Pts',(-1.91199578876737,-1.92965495050268,
6.04612189865165));
#12153=CARTESIAN_POINT('Ctrl Pts',(0.583323960106212,-2.65311689939015,
6.17309210590551));
#12154=CARTESIAN_POINT('Ctrl Pts',(2.54506339572692,-0.949709658787648,
6.30006231315942));
#12155=CARTESIAN_POINT('Ctrl Pts',(2.1787727540419,1.62241961603905,6.42703252041328));
#12156=CARTESIAN_POINT('Ctrl Pts',(-0.180493194875146,2.71048304382584,
6.55400272766719));
#12157=CARTESIAN_POINT('Ctrl Pts',(-2.3746577215157,1.31920310411608,6.68097293492105));
#12158=CARTESIAN_POINT('Ctrl Pts',(-2.39666629782642,-1.27878332063201,
6.80794314217497));
#12159=CARTESIAN_POINT('Ctrl Pts',(-0.226387155107136,-2.70703619855112,
6.93491334942882));
#12160=CARTESIAN_POINT('Ctrl Pts',(2.15097370789069,-1.65909862040404,7.06188355668274));
#12161=CARTESIAN_POINT('Ctrl Pts',(2.560787712971,0.906455963276967,7.18885376393661));
#12162=CARTESIAN_POINT('Ctrl Pts',(0.628188233420324,2.6428536977396,7.3158239711905));
#12163=CARTESIAN_POINT('Ctrl Pts',(-1.87902997824817,1.96177023759366,7.44279417844438));
#12164=CARTESIAN_POINT('Ctrl Pts',(-2.66745473555108,-0.51379116190309,
7.56976438569826));
#12165=CARTESIAN_POINT('Ctrl Pts',(-1.01589514329288,-2.51937555400095,
7.69673459295215));
#12166=CARTESIAN_POINT('Ctrl Pts',(1.56492792151594,-2.22042714915924,7.82370480020605));
#12167=CARTESIAN_POINT('Ctrl Pts',(2.71427416094528,0.109598829776655,7.95067500745992));
#12168=CARTESIAN_POINT('Ctrl Pts',(1.38080920779542,2.33937214994344,8.07764521471382));
#12169=CARTESIAN_POINT('Ctrl Pts',(-1.21571480005839,2.42926607212603,8.20461542196769));
#12170=CARTESIAN_POINT('Ctrl Pts',(-2.70019553829717,0.297052485637893,
8.33158562922158));
#12171=CARTESIAN_POINT('Ctrl Pts',(-1.71474313525672,-2.10688208126453,
8.45855583647548));
#12172=CARTESIAN_POINT('Ctrl Pts',(0.839225635758536,-2.58360145079486,
8.58552604372935));
#12173=CARTESIAN_POINT('Ctrl Pts',(2.62553473866015,-0.697039066589821,
8.71249625098326));
#12174=CARTESIAN_POINT('Ctrl Pts',(2.01020471112819,1.82712154593548,8.83946645823712));
#12175=CARTESIAN_POINT('Ctrl Pts',(-0.443907421755409,2.67997058289342,
8.96643666549102));
#12176=CARTESIAN_POINT('Ctrl Pts',(-2.49196686804545,1.08138672676678,9.0934068727449));
#12177=CARTESIAN_POINT('Ctrl Pts',(-2.26056489494628,-1.50636731244413,
9.22037707999879));
#12178=CARTESIAN_POINT('Ctrl Pts',(0.0386296038606172,-2.71621130952089,
9.34734728725266));
#12179=CARTESIAN_POINT('Ctrl Pts',(2.30248868437777,-1.44147215809947,9.47431749450658));
#12180=CARTESIAN_POINT('Ctrl Pts',(2.46020655093251,1.15181589284589,9.60128770176043));
#12181=CARTESIAN_POINT('Ctrl Pts',(0.367514916265517,2.69151052581742,9.72825790901435));
#12182=CARTESIAN_POINT('Ctrl Pts',(-2.06135136157977,1.76921640518531,9.8552281162682));
#12183=CARTESIAN_POINT('Ctrl Pts',(-2.60465047527895,-0.771422080247088,
9.98219832352212));
#12184=CARTESIAN_POINT('Ctrl Pts',(-0.765413791442057,-2.60642242396238,
10.109168530776));
#12185=CARTESIAN_POINT('Ctrl Pts',(1.77396510930522,-2.05726612649684,10.2361387380299));
#12186=CARTESIAN_POINT('Ctrl Pts',(2.69065589254337,0.373720473328978,10.3631089452838));
#12187=CARTESIAN_POINT('Ctrl Pts',(1.14613967557957,2.46285605919753,10.4900791525376));
#12188=CARTESIAN_POINT('Ctrl Pts',(-1.44677778829329,2.29915857555863,10.6170493597916));
#12189=CARTESIAN_POINT('Ctrl Pts',(-2.71629316639506,0.0323660077726636,
10.7440195670454));
#12190=CARTESIAN_POINT('Ctrl Pts',(-1.50115051956711,-2.26403251784665,
10.8709897742993));
#12191=CARTESIAN_POINT('Ctrl Pts',(1.08713024475642,-2.48946660053905,10.9979599815532));
#12192=CARTESIAN_POINT('Ctrl Pts',(2.68098709335709,-0.437726318053145,
11.1249301888071));
#12193=CARTESIAN_POINT('Ctrl Pts',(1.82248122255242,2.01441264831897,11.251900396061));
#12194=CARTESIAN_POINT('Ctrl Pts',(-0.703091609550923,2.62392040901448,
11.3788706033149));
#12195=CARTESIAN_POINT('Ctrl Pts',(-2.58552980819719,0.833265705034965,
11.5058408105687));
#12196=CARTESIAN_POINT('Ctrl Pts',(-2.10292233868461,-1.71959697653983,
11.6328110178226));
#12197=CARTESIAN_POINT('Ctrl Pts',(0.303278257394332,-2.69950336596484,
11.7597812250765));
#12198=CARTESIAN_POINT('Ctrl Pts',(2.43206301141908,-1.21010976062125,11.8867514323304));
#12199=CARTESIAN_POINT('Ctrl Pts',(2.33618182981621,1.38620005132744,12.0137216395843));
#12200=CARTESIAN_POINT('Ctrl Pts',(0.103339512000114,2.71451967565594,12.1406918468382));
#12201=CARTESIAN_POINT('Ctrl Pts',(-2.224029917602,1.55980352925453,12.267662054092));
#12202=CARTESIAN_POINT('Ctrl Pts',(-2.51702623504576,-1.02170203893063,
12.394632261346));
#12203=CARTESIAN_POINT('Ctrl Pts',(-0.507638733527514,-2.66863242888303,
12.5216024685998));
#12204=CARTESIAN_POINT('Ctrl Pts',(1.96609800268626,-1.87450120514677,12.6485726758537));
#12205=CARTESIAN_POINT('Ctrl Pts',(2.64139808978978,0.634280896384674,12.7755428831076));
#12206=CARTESIAN_POINT('Ctrl Pts',(0.900548461529443,2.56287116193939,12.9025130903615));
#12207=CARTESIAN_POINT('Ctrl Pts',(-1.66405428346344,2.14714216249195,13.0294832976154));
#12208=CARTESIAN_POINT('Ctrl Pts',(-2.70650695994461,-0.232628889080822,
13.1564535048693));
#12209=CARTESIAN_POINT('Ctrl Pts',(-1.27325328751233,-2.39960875771503,
13.2834237121231));
#12210=CARTESIAN_POINT('Ctrl Pts',(1.32467547880323,-2.37160936920924,13.410393919377));
#12211=CARTESIAN_POINT('Ctrl Pts',(2.71089204867564,-0.174242430799153,
13.5373641266309));
#12212=CARTESIAN_POINT('Ctrl Pts',(1.61739112457839,2.18250820717785,13.6643343338848));
#12213=CARTESIAN_POINT('Ctrl Pts',(-0.955575965708573,2.54286663001105,
13.7913045411387));
#12214=CARTESIAN_POINT('Ctrl Pts',(-2.65445497117411,0.577204409436265,
13.9182747483926));
#12215=CARTESIAN_POINT('Ctrl Pts',(-1.92524082103397,-1.91644042570806,
14.0452449556465));
#12216=CARTESIAN_POINT('Ctrl Pts',(0.565036941489686,-2.65707157958072,
14.1722151629003));
#12217=CARTESIAN_POINT('Ctrl Pts',(2.53846196204024,-0.967216103845703,
14.2991853701542));
#12218=CARTESIAN_POINT('Ctrl Pts',(2.18989539383575,1.60737496817656,14.4261555774081));
#12219=CARTESIAN_POINT('Ctrl Pts',(-0.161820625012098,2.71166189072021,
14.553125784662));
#12220=CARTESIAN_POINT('Ctrl Pts',(-2.36551546576707,1.33552712644875,14.6800959919159));
#12221=CARTESIAN_POINT('Ctrl Pts',(-2.40541699517125,-1.26224609470774,
14.8070661991698));
#12222=CARTESIAN_POINT('Ctrl Pts',(-0.245026334360027,-2.70541276328283,
14.9340364064237));
#12223=CARTESIAN_POINT('Ctrl Pts',(2.13949574772732,-1.6738739706801,15.0610066136776));
#12224=CARTESIAN_POINT('Ctrl Pts',(2.56697013530948,0.888797192104508,15.1879768209314));
#12225=CARTESIAN_POINT('Ctrl Pts',(0.646375829365357,2.638464404057,15.3149470281853));
#12226=CARTESIAN_POINT('Ctrl Pts',(-1.86547383569181,1.97466541282641,15.4419172354392));
#12227=CARTESIAN_POINT('Ctrl Pts',(-2.67093017270497,-0.495407041530328,
15.5688874426931));
#12228=CARTESIAN_POINT('Ctrl Pts',(-1.0332230950541,-2.512318881056,15.695857649947));
#12229=CARTESIAN_POINT('Ctrl Pts',(1.54959774514251,-2.23115283038005,15.8228278572008));
#12230=CARTESIAN_POINT('Ctrl Pts',(2.71496463724735,0.0909018303444614,
15.9497980644548));
#12231=CARTESIAN_POINT('Ctrl Pts',(1.39688874166162,2.32980642279196,16.0767682717086));
#12232=CARTESIAN_POINT('Ctrl Pts',(-1.19895454105405,2.43758161560788,16.2037384789625));
#12233=CARTESIAN_POINT('Ctrl Pts',(-2.69808556207027,0.315642874165645,
16.3307086862164));
#12234=CARTESIAN_POINT('Ctrl Pts',(-1.72921348729331,-2.09502191865062,
16.4576788934703));
#12235=CARTESIAN_POINT('Ctrl Pts',(0.821411330955809,-2.58932028718755,
16.5846491007242));
#12236=CARTESIAN_POINT('Ctrl Pts',(2.62067164979186,-0.715105746194832,
16.7116193079781));
#12237=CARTESIAN_POINT('Ctrl Pts',(2.02274122135563,1.81323304505856,16.838589515232));
#12238=CARTESIAN_POINT('Ctrl Pts',(-0.425438756788597,2.6829644031343,16.9655597224858));
#12239=CARTESIAN_POINT('Ctrl Pts',(-2.48445977586001,1.09852434947853,17.0925299297397));
#12240=CARTESIAN_POINT('Ctrl Pts',(-2.27088629148237,-1.49076207874399,
17.2195001369936));
#12241=CARTESIAN_POINT('Ctrl Pts',(0.0199209457316412,-2.716412943605,17.3464703442475));
#12242=CARTESIAN_POINT('Ctrl Pts',(2.29250601963548,-1.45729622047088,17.4734405515014));
#12243=CARTESIAN_POINT('Ctrl Pts',(2.46808126066971,1.134844048755,17.6004107587553));
#12244=CARTESIAN_POINT('Ctrl Pts',(0.386043816015746,2.68891544983839,17.7273809660092));
#12245=CARTESIAN_POINT('Ctrl Pts',(-2.04911709752763,1.78337187509604,17.854351173263));
#12246=CARTESIAN_POINT('Ctrl Pts',(-2.60990181950929,-0.753464409767162,
17.9813213805169));
#12247=CARTESIAN_POINT('Ctrl Pts',(-0.783347214370861,-2.60108886161181,
18.1082915877708));
#12248=CARTESIAN_POINT('Ctrl Pts',(1.75975373656424,-2.06943540873153,18.2352617950247));
#12249=CARTESIAN_POINT('Ctrl Pts',(2.69316605096044,0.355179878678,18.3622320022786));
#12250=CARTESIAN_POINT('Ctrl Pts',(1.16307526349234,2.45490367544551,18.4892022095325));
#12251=CARTESIAN_POINT('Ctrl Pts',(-1.43090815632692,2.30906863744254,18.6161724167864));
#12252=CARTESIAN_POINT('Ctrl Pts',(-2.71600582053626,0.0510735457626923,
18.7431426240402));
#12253=CARTESIAN_POINT('Ctrl Pts',(-1.51670830191366,-2.25363973411232,
18.8701128312942));
#12254=CARTESIAN_POINT('Ctrl Pts',(1.0699584080944,-2.49689509775876,18.997083038548));
#12255=CARTESIAN_POINT('Ctrl Pts',(2.67790869017686,-0.456181072972995,
19.1240532458019));
#12256=CARTESIAN_POINT('Ctrl Pts',(1.83631214152924,2.00181263936867,19.2510234530558));
#12257=CARTESIAN_POINT('Ctrl Pts',(-0.685002839272038,2.62870067418348,
19.3779936603097));
#12258=CARTESIAN_POINT('Ctrl Pts',(-2.57972941542172,0.85105362197164,19.5049638675636));
#12259=CARTESIAN_POINT('Ctrl Pts',(-2.11471608077217,-1.70507243892711,
19.6319340748175));
#12260=CARTESIAN_POINT('Ctrl Pts',(0.284678397100628,-2.70152814800923,
19.7589042820713));
#12261=CARTESIAN_POINT('Ctrl Pts',(2.4236707679272,-1.22683174598488,19.8858744893252));
#12262=CARTESIAN_POINT('Ctrl Pts',(2.34567378804177,1.37007686075223,20.0128446965791));
#12263=CARTESIAN_POINT('Ctrl Pts',(0.122033151777428,2.71374354612161,20.139814903833));
#12264=CARTESIAN_POINT('Ctrl Pts',(-2.21323411359773,1.57508440493182,20.2667851110869));
#12265=CARTESIAN_POINT('Ctrl Pts',(-2.52400344576924,-1.00434193882558,
20.3937553183407));
#12266=CARTESIAN_POINT('Ctrl Pts',(-0.526006738186656,-2.6650728011692,
20.5207255255947));
#12267=CARTESIAN_POINT('Ctrl Pts',(1.95314085515653,-1.88799812609669,20.6476957328485));
#12268=CARTESIAN_POINT('Ctrl Pts',(2.64570401084464,0.616073381793945,20.7746659401024));
#12269=CARTESIAN_POINT('Ctrl Pts',(0.918178722395619,2.55660790054414,20.9016361473563));
#12270=CARTESIAN_POINT('Ctrl Pts',(-1.64922650159215,2.1585523090131,21.0286063546102));
#12271=CARTESIAN_POINT('Ctrl Pts',(-2.70804498314286,-0.213982468094741,
21.1555765618641));
#12272=CARTESIAN_POINT('Ctrl Pts',(-1.28975024744425,-2.39078238593873,
21.282546769118));
#12273=CARTESIAN_POINT('Ctrl Pts',(1.30830974050215,-2.38067674190542,21.4095169763718));
#12274=CARTESIAN_POINT('Ctrl Pts',(2.7096276693385,-0.192909400827225,21.5364871836258));
#12275=CARTESIAN_POINT('Ctrl Pts',(1.63238464894961,2.17131675127667,21.6634573908796));
#12276=CARTESIAN_POINT('Ctrl Pts',(-0.938039446297698,2.54938779923009,
21.7904275981335));
#12277=CARTESIAN_POINT('Ctrl Pts',(-2.65041657616178,0.595473097237805,
21.9173978053874));
#12278=CARTESIAN_POINT('Ctrl Pts',(-1.93839447572803,-1.90313495096593,
22.0443680126413));
#12279=CARTESIAN_POINT('Ctrl Pts',(0.546723025340935,-2.66090028954102,
22.1713382198951));
#12280=CARTESIAN_POINT('Ctrl Pts',(2.5317402887165,-0.984676525168914,22.2983084271491));
#12281=CARTESIAN_POINT('Ctrl Pts',(2.20091381098623,1.59225380109178,22.4252786344029));
#12282=CARTESIAN_POINT('Ctrl Pts',(-0.143139731775406,2.71271261682962,
22.5522488416569));
#12283=CARTESIAN_POINT('Ctrl Pts',(-2.3562622284463,1.35178681709819,22.6792190489107));
#12284=CARTESIAN_POINT('Ctrl Pts',(-2.41405123879661,-1.24564712890483,
22.8061892561647));
#12285=CARTESIAN_POINT('Ctrl Pts',(-0.263658360263974,-2.7036645370246,
22.9331594634184));
#12286=CARTESIAN_POINT('Ctrl Pts',(2.12792480902252,-1.68856316174379,23.0601296706724));
#12287=CARTESIAN_POINT('Ctrl Pts',(2.57301457260841,0.871083393326757,23.1870998779262));
#12288=CARTESIAN_POINT('Ctrl Pts',(0.664563645007867,2.63397445159584,23.3140700851802));
#12289=CARTESIAN_POINT('Ctrl Pts',(-1.85188801762549,1.98742024690464,23.441040292434));
#12290=CARTESIAN_POINT('Ctrl Pts',(-2.67416688047444,-0.476910534840453,
23.5680104996879));
#12291=CARTESIAN_POINT('Ctrl Pts',(-1.05071544021771,-2.50531234164241,
23.6949807069418));
#12292=CARTESIAN_POINT('Ctrl Pts',(1.53460087730742,-2.24145001013409,23.8219509141957));
#12293=CARTESIAN_POINT('Ctrl Pts',(2.71474831193969,0.0715842898877685,
23.9489211214496));
#12294=CARTESIAN_POINT('Ctrl Pts',(1.4144115015539,2.3213185430733,24.0758913287035));
#12295=CARTESIAN_POINT('Ctrl Pts',(-1.18525106712396,2.44339045977451,24.2028615359573));
#12296=CARTESIAN_POINT('Ctrl Pts',(-2.18711439872577,1.04106308798187,24.2875083407933));
#12297=CARTESIAN_POINT('Ctrl Pts',(-2.28111993934175,0.282802338419006,
24.3298317432112));
#12298=CARTESIAN_POINT('Ctrl Pts',(1.24871913126432,-1.7461037509244,-0.0877091283943906));
#12299=CARTESIAN_POINT('Ctrl Pts',(1.82913663415658,-1.33102048934929,-0.0453857259764285));
#12300=CARTESIAN_POINT('Ctrl Pts',(2.53354408385517,0.116190684323019,0.0392610788594953));
#12301=CARTESIAN_POINT('Ctrl Pts',(1.27477413639151,2.19535803865958,0.166231286113382));
#12302=CARTESIAN_POINT('Ctrl Pts',(-1.15112416905651,2.25992566216479,0.293201493367268));
#12303=CARTESIAN_POINT('Ctrl Pts',(-2.52350313926065,0.260522656942532,
0.420171700621154));
#12304=CARTESIAN_POINT('Ctrl Pts',(-1.58786719865054,-1.97886879483645,
0.54714190787504));
#12305=CARTESIAN_POINT('Ctrl Pts',(0.800382785444057,-2.40726064333533,
0.674112115128925));
#12306=CARTESIAN_POINT('Ctrl Pts',(2.45642266052488,-0.634136319309549,
0.801082322382812));
#12307=CARTESIAN_POINT('Ctrl Pts',(1.86555673694162,1.71929037441,0.928052529636697));
#12308=CARTESIAN_POINT('Ctrl Pts',(-0.431800654848601,2.49991376216546,
1.05502273689058));
#12309=CARTESIAN_POINT('Ctrl Pts',(-2.33416799486367,0.993873445412137,
1.18199294414447));
#12310=CARTESIAN_POINT('Ctrl Pts',(-2.10142245142702,-1.42132171331109,
1.30896315139835));
#12311=CARTESIAN_POINT('Ctrl Pts',(0.0535474650605221,-2.53638161334886,
1.43593335865224));
#12312=CARTESIAN_POINT('Ctrl Pts',(2.15953454504651,-1.33136255670197,1.56290356590613));
#12313=CARTESIAN_POINT('Ctrl Pts',(2.29014485575358,1.09149061223455,1.68987377316002));
#12314=CARTESIAN_POINT('Ctrl Pts',(0.325904679009007,2.51592866283334,1.8168439804139));
#12315=CARTESIAN_POINT('Ctrl Pts',(-1.9364480208908,1.63898827214785,1.94381418766779));
#12316=CARTESIAN_POINT('Ctrl Pts',(-2.42748574474482,-0.737174446015656,
2.07078439492167));
#12317=CARTESIAN_POINT('Ctrl Pts',(-0.698044400113263,-2.43902576224114,
2.19775460217556));
#12318=CARTESIAN_POINT('Ctrl Pts',(1.66991473982413,-1.90984235187298,2.32472480942945));
#12319=CARTESIAN_POINT('Ctrl Pts',(2.51036313095016,0.36631943112233,2.45169501668333));
#12320=CARTESIAN_POINT('Ctrl Pts',(1.05452259326343,2.3074000537054,2.57866522393722));
#12321=CARTESIAN_POINT('Ctrl Pts',(-1.36591485990746,2.13784694525844,2.7056354311911));
#12322=CARTESIAN_POINT('Ctrl Pts',(-2.53691747567054,0.012754325751266,
2.832605638445));
#12323=CARTESIAN_POINT('Ctrl Pts',(-1.38734127971241,-2.1240049710581,2.95957584569887));
#12324=CARTESIAN_POINT('Ctrl Pts',(1.03126901189414,-2.31788635981642,3.08654605295276));
#12325=CARTESIAN_POINT('Ctrl Pts',(2.50655298773216,-0.391541912089928,
3.21351626020665));
#12326=CARTESIAN_POINT('Ctrl Pts',(1.68903327305286,1.89295524272351,3.34048646746053));
#12327=CARTESIAN_POINT('Ctrl Pts',(-0.673485386471964,2.44592117285849,
3.46745667471442));
#12328=CARTESIAN_POINT('Ctrl Pts',(-2.41995092966926,0.761544776858728,
3.5944268819683));
#12329=CARTESIAN_POINT('Ctrl Pts',(-1.95282974673297,-1.61943475613438,
3.7213970892222));
#12330=CARTESIAN_POINT('Ctrl Pts',(0.300591295705853,-2.51907876459076,
3.84836729647607));
#12331=CARTESIAN_POINT('Ctrl Pts',(2.27905432392247,-1.11446145639985,3.97533750372997));
#12332=CARTESIAN_POINT('Ctrl Pts',(2.17281210557263,1.30958027744207,4.10230771098385));
#12333=CARTESIAN_POINT('Ctrl Pts',(0.0790469270504698,2.53571775490379,
4.22927791823773));
#12334=CARTESIAN_POINT('Ctrl Pts',(-2.08702435748228,1.44237383520157,4.35624812549163));
#12335=CARTESIAN_POINT('Ctrl Pts',(-2.34404477733026,-0.970343769532158,
4.4832183327455));
#12336=CARTESIAN_POINT('Ctrl Pts',(-0.456911635684403,-2.49546482771812,
4.6101885399994));
#12337=CARTESIAN_POINT('Ctrl Pts',(1.84816945662178,-1.73792479952687,4.73715874725328));
#12338=CARTESIAN_POINT('Ctrl Pts',(2.46268594837716,0.609336416822525,4.86412895450717));
#12339=CARTESIAN_POINT('Ctrl Pts',(0.824524975042275,2.39922310649351,4.99109916176105));
#12340=CARTESIAN_POINT('Ctrl Pts',(-1.56784862207678,1.99448330337771,5.11806936901495));
#12341=CARTESIAN_POINT('Ctrl Pts',(-2.52607375948148,-0.234657859147452,
5.24503957626882));
#12342=CARTESIAN_POINT('Ctrl Pts',(-1.1736390919323,-2.24915189151133,5.37200978352272));
#12343=CARTESIAN_POINT('Ctrl Pts',(1.25235119333062,-2.20629314411389,5.49897999077659));
#12344=CARTESIAN_POINT('Ctrl Pts',(2.53278602786547,-0.145285533519461,
5.62595019803048));
#12345=CARTESIAN_POINT('Ctrl Pts',(1.49642118575949,2.0486182133357,5.75292040528437));
#12346=CARTESIAN_POINT('Ctrl Pts',(-0.908755739619028,2.36860210987622,
5.87989061253825));
#12347=CARTESIAN_POINT('Ctrl Pts',(-2.4826721556093,0.521969268216885,6.00686081979214));
#12348=CARTESIAN_POINT('Ctrl Pts',(-1.78562924695095,-1.80212128937927,
6.13383102704603));
#12349=CARTESIAN_POINT('Ctrl Pts',(0.544771243604218,-2.47776860125043,
6.26080123429992));
#12350=CARTESIAN_POINT('Ctrl Pts',(2.3768565084989,-0.886941986381852,6.3877714415538));
#12351=CARTESIAN_POINT('Ctrl Pts',(2.03477454026465,1.51519157847824,6.51474164880769));
#12352=CARTESIAN_POINT('Ctrl Pts',(-0.168564140955765,2.53134333498726,
6.64171185606157));
#12353=CARTESIAN_POINT('Ctrl Pts',(-2.21771318950963,1.23201508037672,6.76868206331545));
#12354=CARTESIAN_POINT('Ctrl Pts',(-2.23826718747087,-1.19426669830983,
6.89565227056935));
#12355=CARTESIAN_POINT('Ctrl Pts',(-0.211424903584118,-2.52812429665652,
7.02262247782322));
#12356=CARTESIAN_POINT('Ctrl Pts',(2.00881277291316,-1.54944641487905,7.14959268507712));
#12357=CARTESIAN_POINT('Ctrl Pts',(2.39154158308137,0.846546989595545,7.276562892331));
#12358=CARTESIAN_POINT('Ctrl Pts',(0.586670372798765,2.46818370930543,7.40353309958489));
#12359=CARTESIAN_POINT('Ctrl Pts',(-1.75484219409317,1.83211403112111,7.53050330683878));
#12360=CARTESIAN_POINT('Ctrl Pts',(-2.49115882927151,-0.479833967683821,
7.65747351409266));
#12361=CARTESIAN_POINT('Ctrl Pts',(-0.94875317736379,-2.35286641304659,
7.78444372134655));
#12362=CARTESIAN_POINT('Ctrl Pts',(1.46149959243917,-2.07367593671256,7.91141392860043));
#12363=CARTESIAN_POINT('Ctrl Pts',(2.53488389174312,0.102355286047412,8.03838413585432));
#12364=CARTESIAN_POINT('Ctrl Pts',(1.28954954837439,2.18475969193136,8.16535434310821));
#12365=CARTESIAN_POINT('Ctrl Pts',(-1.13536646664624,2.26871239596733,8.29232455036209));
#12366=CARTESIAN_POINT('Ctrl Pts',(-2.52173574544231,0.277419861147555,
8.41929475761597));
#12367=CARTESIAN_POINT('Ctrl Pts',(-1.60141330399934,-1.96763522507972,
8.54626496486987));
#12368=CARTESIAN_POINT('Ctrl Pts',(0.783760010772541,-2.41284752827741,
8.67323517212374));
#12369=CARTESIAN_POINT('Ctrl Pts',(2.45200938505186,-0.65097075573196,8.80020537937764));
#12370=CARTESIAN_POINT('Ctrl Pts',(1.87734740088688,1.70636446446352,8.92717558663151));
#12371=CARTESIAN_POINT('Ctrl Pts',(-0.414568944074917,2.50284748632617,
9.05414579388541));
#12372=CARTESIAN_POINT('Ctrl Pts',(-2.32726920642608,1.00991632822801,9.18111600113929));
#12373=CARTESIAN_POINT('Ctrl Pts',(-2.11116092135796,-1.40680933794583,
9.30808620839318));
#12374=CARTESIAN_POINT('Ctrl Pts',(0.0360765179802292,-2.53669301139319,
9.43505641564706));
#12375=CARTESIAN_POINT('Ctrl Pts',(2.15031390746369,-1.34620319735501,9.56202662290096));
#12376=CARTESIAN_POINT('Ctrl Pts',(2.2976079741878,1.0756907297868,9.68899683015483));
#12377=CARTESIAN_POINT('Ctrl Pts',(0.343225328753236,2.51362473788409,9.81596703740874));
#12378=CARTESIAN_POINT('Ctrl Pts',(-1.92511369591032,1.65228635745112,9.94293724466261));
#12379=CARTESIAN_POINT('Ctrl Pts',(-2.43250539256738,-0.720437689416097,
10.0699074519165));
#12380=CARTESIAN_POINT('Ctrl Pts',(-0.714826497028901,-2.43416023062287,
10.1968776591704));
#12381=CARTESIAN_POINT('Ctrl Pts',(1.65672121291019,-1.92129845986873,10.3238478664243));
#12382=CARTESIAN_POINT('Ctrl Pts',(2.51282658854792,0.34902075165695,10.4508180736782));
#12383=CARTESIAN_POINT('Ctrl Pts',(1.07038966185442,2.30008237265446,10.577788280932));
#12384=CARTESIAN_POINT('Ctrl Pts',(-1.35115817084561,2.14720389030891,10.7047584881859));
#12385=CARTESIAN_POINT('Ctrl Pts',(-2.53676945822922,0.0302268919343324,
10.8317286954398));
#12386=CARTESIAN_POINT('Ctrl Pts',(-1.40193733038645,-2.11439936409126,
10.9586989026937));
#12387=CARTESIAN_POINT('Ctrl Pts',(1.01528024888245,-2.3249341851824,11.0856691099476));
#12388=CARTESIAN_POINT('Ctrl Pts',(2.50379681415649,-0.40879635837472,11.2126393172015));
#12389=CARTESIAN_POINT('Ctrl Pts',(1.70203082670308,1.88127722947816,11.3396095244553));
#12390=CARTESIAN_POINT('Ctrl Pts',(-0.656623277454625,2.45050174876602,
11.4665797317093));
#12391=CARTESIAN_POINT('Ctrl Pts',(-2.41464843777542,0.778193980411903,
11.5935499389631));
#12392=CARTESIAN_POINT('Ctrl Pts',(-1.96393718756176,-1.60594634795581,
11.720520146217));
#12393=CARTESIAN_POINT('Ctrl Pts',(0.283234162726211,-2.52108931977139,
11.8474903534709));
#12394=CARTESIAN_POINT('Ctrl Pts',(2.2713244815341,-1.1301318722983,11.9744605607248));
#12395=CARTESIAN_POINT('Ctrl Pts',(2.18178022463351,1.29458410333155,12.1014307679787));
#12396=CARTESIAN_POINT('Ctrl Pts',(0.0965096555531949,2.53511318003469,
12.2284009752326));
#12397=CARTESIAN_POINT('Ctrl Pts',(-2.07704059302567,1.45671387860629,12.3553711824864));
#12398=CARTESIAN_POINT('Ctrl Pts',(-2.35067236394805,-0.954176286946753,
12.4823413897403));
#12399=CARTESIAN_POINT('Ctrl Pts',(-0.474088162116868,-2.49225868716336,
12.6093115969942));
#12400=CARTESIAN_POINT('Ctrl Pts',(1.83615576801644,-1.75061273409641,12.7362818042481));
#12401=CARTESIAN_POINT('Ctrl Pts',(2.46682430457111,0.59236036293617,12.863252011502));
#12402=CARTESIAN_POINT('Ctrl Pts',(0.841029923104784,2.39348733392156,12.9902222187559));
#12403=CARTESIAN_POINT('Ctrl Pts',(-1.55407455106469,2.00523445984096,13.1171924260098));
#12404=CARTESIAN_POINT('Ctrl Pts',(-2.52763003618799,-0.217254112414209,
13.2441626332636));
#12405=CARTESIAN_POINT('Ctrl Pts',(-1.18910215300433,-2.24101517596849,
13.3711328405175));
#12406=CARTESIAN_POINT('Ctrl Pts',(1.23712577797812,-2.21486630717581,13.4981030477714));
#12407=CARTESIAN_POINT('Ctrl Pts',(2.53172530812039,-0.16272649883577,13.6250732550253));
#12408=CARTESIAN_POINT('Ctrl Pts',(1.51049542722474,2.03826311194943,13.7520434622792));
#12409=CARTESIAN_POINT('Ctrl Pts',(-0.892420580671138,2.37480493017746,
13.8790136695331));
#12410=CARTESIAN_POINT('Ctrl Pts',(-2.47901823795254,0.539056142808217,
14.0059838767869));
#12411=CARTESIAN_POINT('Ctrl Pts',(-1.79799889605321,-1.78978013146645,
14.1329540840409));
#12412=CARTESIAN_POINT('Ctrl Pts',(0.527692840255718,-2.48146191095963,
14.2599242912947));
#12413=CARTESIAN_POINT('Ctrl Pts',(2.37069137302528,-0.903291405397025,
14.3868944985486));
#12414=CARTESIAN_POINT('Ctrl Pts',(2.04516206885435,1.5011412529539,14.5138647058025));
#12415=CARTESIAN_POINT('Ctrl Pts',(-0.151125667995169,2.53244427020094,
14.6408349130564));
#12416=CARTESIAN_POINT('Ctrl Pts',(-2.20917515854546,1.24726022467899,14.7678051203103));
#12417=CARTESIAN_POINT('Ctrl Pts',(-2.2464395386873,-1.17882244134687,14.8947753275642));
#12418=CARTESIAN_POINT('Ctrl Pts',(-0.228832192767835,-2.5266081565517,
15.0217455348181));
#12419=CARTESIAN_POINT('Ctrl Pts',(1.99809340758638,-1.56324524108038,15.1487157420719));
#12420=CARTESIAN_POINT('Ctrl Pts',(2.39731540026729,0.830055311917173,15.2756859493258));
#12421=CARTESIAN_POINT('Ctrl Pts',(0.603655924462618,2.46408451033275,15.4026561565797));
#12422=CARTESIAN_POINT('Ctrl Pts',(-1.74218199642607,1.84415694574227,15.5296263638336));
#12423=CARTESIAN_POINT('Ctrl Pts',(-2.49440456980315,-0.462664880173312,
15.6565965710875));
#12424=CARTESIAN_POINT('Ctrl Pts',(-0.964935899959919,-2.34627612572969,
15.7835667783414));
#12425=CARTESIAN_POINT('Ctrl Pts',(1.44718260939238,-2.0836927422902,15.9105369855953));
#12426=CARTESIAN_POINT('Ctrl Pts',(2.53552873347685,0.0848939981029082,
16.0375071928491));
#12427=CARTESIAN_POINT('Ctrl Pts',(1.30456636280332,2.17582617739623,16.164477400103));
#12428=CARTESIAN_POINT('Ctrl Pts',(-1.11971391717911,2.27647835326322,16.2914476073569));
#12429=CARTESIAN_POINT('Ctrl Pts',(-2.51976522056811,0.294781584255081,
16.4184178146108));
#12430=CARTESIAN_POINT('Ctrl Pts',(-1.61492728973195,-1.95655891761011,
16.5453880218647));
#12431=CARTESIAN_POINT('Ctrl Pts',(0.767123078904428,-2.41818839857708,
16.6723582291185));
#12432=CARTESIAN_POINT('Ctrl Pts',(2.4474677046963,-0.667843382589994,16.7993284363725));
#12433=CARTESIAN_POINT('Ctrl Pts',(1.88905535518695,1.69339387451358,16.9262986436263));
#12434=CARTESIAN_POINT('Ctrl Pts',(-0.397320899643744,2.5056434406968,17.0532688508803));
#12435=CARTESIAN_POINT('Ctrl Pts',(-2.32025826872181,1.02592130089431,17.1802390581341));
#12436=CARTESIAN_POINT('Ctrl Pts',(-2.12080016200509,-1.39223547650525,
17.307209265388));
#12437=CARTESIAN_POINT('Ctrl Pts',(0.0186043418789166,-2.53688131919171,
17.4341794726419));
#12438=CARTESIAN_POINT('Ctrl Pts',(2.14099101134067,-1.36098142476636,17.5611496798958));
#12439=CARTESIAN_POINT('Ctrl Pts',(2.30496223307299,1.05984057919471,17.6881198871497));
#12440=CARTESIAN_POINT('Ctrl Pts',(0.360529626964672,2.51120117419559,17.8150900944035));
#12441=CARTESIAN_POINT('Ctrl Pts',(-1.91368801190267,1.66550627206883,17.9420603016574));
#12442=CARTESIAN_POINT('Ctrl Pts',(-2.43740966793167,-0.703666867113844,
18.0690305089113));
#12443=CARTESIAN_POINT('Ctrl Pts',(-0.731574674335433,-2.42917917105174,
18.1960007161652));
#12444=CARTESIAN_POINT('Ctrl Pts',(1.64344909016039,-1.93266345680038,18.3229709234191));
#12445=CARTESIAN_POINT('Ctrl Pts',(2.51517084699783,0.33170553147752,18.449941130673));
#12446=CARTESIAN_POINT('Ctrl Pts',(1.08620595249116,2.2926555733414,18.5769113379269));
#12447=CARTESIAN_POINT('Ctrl Pts',(-1.33633738559912,2.15645898200052,18.7038815451807));
#12448=CARTESIAN_POINT('Ctrl Pts',(-2.53650110347004,0.0476980219282782,
18.8308517524346));
#12449=CARTESIAN_POINT('Ctrl Pts',(-1.41646687660141,-2.10469345432813,
18.9578219596885));
#12450=CARTESIAN_POINT('Ctrl Pts',(0.999243323514884,-2.33187172237487,
19.0847921669424));
#12451=CARTESIAN_POINT('Ctrl Pts',(2.50092186705419,-0.426031412093869,
19.2117623741963));
#12452=CARTESIAN_POINT('Ctrl Pts',(1.71494764042323,1.86950997317682,19.3387325814502));
#12453=CARTESIAN_POINT('Ctrl Pts',(-0.639730019927018,2.45496607935927,
19.4657027887041));
#12454=CARTESIAN_POINT('Ctrl Pts',(-2.40923140127119,0.794806268425853,
19.592672995958));
#12455=CARTESIAN_POINT('Ctrl Pts',(-1.97495146433281,-1.59238175784946,
19.7196432032118));
#12456=CARTESIAN_POINT('Ctrl Pts',(0.265863593855321,-2.52298028106869,
19.8466134104657));
#12457=CARTESIAN_POINT('Ctrl Pts',(2.26348689344177,-1.14574867768449,19.9735836177196));
#12458=CARTESIAN_POINT('Ctrl Pts',(2.19064484573673,1.27952651752807,20.1005538249735));
#12459=CARTESIAN_POINT('Ctrl Pts',(0.113967805887229,2.53438834601358,20.2275240322274));
#12460=CARTESIAN_POINT('Ctrl Pts',(-2.06695829917982,1.47098481931061,20.3544942394812));
#12461=CARTESIAN_POINT('Ctrl Pts',(-2.35718844081557,-0.93796354073691,
20.4814644467352));
#12462=CARTESIAN_POINT('Ctrl Pts',(-0.491242199024368,-2.48893432034654,
20.608434653989));
#12463=CARTESIAN_POINT('Ctrl Pts',(1.82405497693622,-1.76321762419793,20.7354048612429));
#12464=CARTESIAN_POINT('Ctrl Pts',(2.47084564113251,0.575356209078461,20.8623750684968));
#12465=CARTESIAN_POINT('Ctrl Pts',(0.857494974763876,2.38763802044798,20.9893452757507));
#12466=CARTESIAN_POINT('Ctrl Pts',(-1.5402267585474,2.01589049342632,21.1163154830046));
#12467=CARTESIAN_POINT('Ctrl Pts',(-2.52906640922887,-0.199840060113828,
21.2432856902585));
#12468=CARTESIAN_POINT('Ctrl Pts',(-1.20450880521207,-2.23277215175221,
21.3702558975124));
#12469=CARTESIAN_POINT('Ctrl Pts',(1.22184167477557,-2.22333440421579,21.4972261047662));
#12470=CARTESIAN_POINT('Ctrl Pts',(2.53054449342564,-0.180159742062507,
21.6241963120202));
#12471=CARTESIAN_POINT('Ctrl Pts',(1.52449800808261,2.02781131540755,21.751166519274));
#12472=CARTESIAN_POINT('Ctrl Pts',(-0.876043074960227,2.38089510597715,
21.8781367265279));
#12473=CARTESIAN_POINT('Ctrl Pts',(-2.47524674625411,0.556117426851564,
22.0051069337818));
#12474=CARTESIAN_POINT('Ctrl Pts',(-1.81028320685765,-1.77735403461849,
22.1320771410357));
#12475=CARTESIAN_POINT('Ctrl Pts',(0.510589317071444,-2.48503757599162,
22.2590473482895));
#12476=CARTESIAN_POINT('Ctrl Pts',(2.36441394472454,-0.919597842451947,
22.3860175555435));
#12477=CARTESIAN_POINT('Ctrl Pts',(2.05545226302454,1.48701946547234,22.5129877627973));
#12478=CARTESIAN_POINT('Ctrl Pts',(-0.133679421764624,2.53342555231595,
22.6399579700512));
#12479=CARTESIAN_POINT('Ctrl Pts',(-2.2005334809403,1.26244528907117,22.7669281773051));
#12480=CARTESIAN_POINT('Ctrl Pts',(-2.25450313277747,-1.16332052498233,
22.893898384559));
#12481=CARTESIAN_POINT('Ctrl Pts',(-0.24623280137769,-2.52497547307231,
23.0208685918128));
#12482=CARTESIAN_POINT('Ctrl Pts',(1.98728720880323,-1.57696360245516,23.1478387990668));
#12483=CARTESIAN_POINT('Ctrl Pts',(2.40296035204267,0.813512243486801,23.2748090063206));
#12484=CARTESIAN_POINT('Ctrl Pts',(0.620641681303831,2.45989130526442,23.4017792135745));
#12485=CARTESIAN_POINT('Ctrl Pts',(-1.72949408454599,1.85606879455694,23.5287494208284));
#12486=CARTESIAN_POINT('Ctrl Pts',(-2.49742735891751,-0.445390834118454,
23.6557196280823));
#12487=CARTESIAN_POINT('Ctrl Pts',(-0.981272150962877,-2.33973265854723,
23.7826898353362));
#12488=CARTESIAN_POINT('Ctrl Pts',(1.43317690604497,-2.0933093666771,23.9096600425901));
#12489=CARTESIAN_POINT('Ctrl Pts',(2.53532670541879,0.0668531815795256,
24.036630249844));
#12490=CARTESIAN_POINT('Ctrl Pts',(1.32093101838195,2.16789927381241,24.1636004570979));
#12491=CARTESIAN_POINT('Ctrl Pts',(-1.10691612547992,2.28190328259405,24.2905706643517));
#12492=CARTESIAN_POINT('Ctrl Pts',(-2.04256487369668,0.972257736519369,
24.3752174691877));
#12493=CARTESIAN_POINT('Ctrl Pts',(-2.13035745341128,0.264111526580659,
24.4175408716056));
#12494=CARTESIAN_POINT('Ctrl Pts',(1.160348984669,-1.62253437445178,0.));
#12495=CARTESIAN_POINT('Ctrl Pts',(1.69969113399867,-1.23682598810383,0.0423234024179621));
#12496=CARTESIAN_POINT('Ctrl Pts',(2.35424863102644,0.107968028363325,0.126970207253886));
#12497=CARTESIAN_POINT('Ctrl Pts',(1.18456011268651,2.03999555013175,0.253940414507772));
#12498=CARTESIAN_POINT('Ctrl Pts',(-1.06966068457706,2.09999381115058,0.380910621761658));
#12499=CARTESIAN_POINT('Ctrl Pts',(-2.34491827036033,0.242085824504435,
0.507880829015544));
#12500=CARTESIAN_POINT('Ctrl Pts',(-1.47549600675849,-1.83882695427017,
0.634851036269431));
#12501=CARTESIAN_POINT('Ctrl Pts',(0.743740789408913,-2.23690209703098,
0.761821243523316));
#12502=CARTESIAN_POINT('Ctrl Pts',(2.28258498544192,-0.589259358513722,
0.888791450777202));
#12503=CARTESIAN_POINT('Ctrl Pts',(1.73353383587625,1.59761854395386,1.01576165803109));
#12504=CARTESIAN_POINT('Ctrl Pts',(-0.401242712543095,2.32299828124824,
1.14273186528497));
#12505=CARTESIAN_POINT('Ctrl Pts',(-2.16898211541349,0.923538379768288,
1.26970207253886));
#12506=CARTESIAN_POINT('Ctrl Pts',(-1.95270765604849,-1.32073671783877,
1.39667227979275));
#12507=CARTESIAN_POINT('Ctrl Pts',(0.0497579841286025,-2.35688535243524,
1.52364248704663));
#12508=CARTESIAN_POINT('Ctrl Pts',(2.00670723621032,-1.23714384781738,1.65061269430052));
#12509=CARTESIAN_POINT('Ctrl Pts',(2.1280744337024,1.01424731308453,1.77758290155441));
#12510=CARTESIAN_POINT('Ctrl Pts',(0.302840850211159,2.33787982927957,1.90455310880829));
#12511=CARTESIAN_POINT('Ctrl Pts',(-1.79940824053038,1.52299931173928,2.03152331606218));
#12512=CARTESIAN_POINT('Ctrl Pts',(-2.25569589565051,-0.685005617790214,
2.15849352331606));
#12513=CARTESIAN_POINT('Ctrl Pts',(-0.648644751766769,-2.26641924187756,
2.28546373056995));
#12514=CARTESIAN_POINT('Ctrl Pts',(1.55173715555782,-1.77468541835342,2.41243393782384));
#12515=CARTESIAN_POINT('Ctrl Pts',(2.33270816248269,0.340395505542482,2.53940414507772));
#12516=CARTESIAN_POINT('Ctrl Pts',(0.979895470300759,2.14410850487368,2.66637435233161));
#12517=CARTESIAN_POINT('Ctrl Pts',(-1.2692509317393,1.98655443822406,2.7933445595855));
#12518=CARTESIAN_POINT('Ctrl Pts',(-2.35738329251264,0.0118517195461532,
2.92031476683938));
#12519=CARTESIAN_POINT('Ctrl Pts',(-1.28916103309304,-1.97369204162334,
3.04728497409327));
#12520=CARTESIAN_POINT('Ctrl Pts',(0.958287513109827,-2.15385270943036,
3.17425518134715));
#12521=CARTESIAN_POINT('Ctrl Pts',(2.32916765789381,-0.363833025997572,
3.30122538860104));
#12522=CARTESIAN_POINT('Ctrl Pts',(1.56950269631471,1.75899338684286,3.42819559585493));
#12523=CARTESIAN_POINT('Ctrl Pts',(-0.6258237459619,2.27282667370784,3.55516580310881));
#12524=CARTESIAN_POINT('Ctrl Pts',(-2.24869430914181,0.70765129362066,3.68213601036269));
#12525=CARTESIAN_POINT('Ctrl Pts',(-1.8146306540197,-1.50482957133494,3.80910621761659));
#12526=CARTESIAN_POINT('Ctrl Pts',(0.279318860454586,-2.34080700264011,
3.93607642487046));
#12527=CARTESIAN_POINT('Ctrl Pts',(2.11776876365419,-1.03559254199705,4.06304663212436));
#12528=CARTESIAN_POINT('Ctrl Pts',(2.01904516192129,1.21690307069604,4.19001683937824));
#12529=CARTESIAN_POINT('Ctrl Pts',(0.0734528840375746,2.35626847434518,
4.31698704663213));
#12530=CARTESIAN_POINT('Ctrl Pts',(-1.93932849553776,1.34029900983,4.44395725388601));
#12531=CARTESIAN_POINT('Ctrl Pts',(-2.17815993148116,-0.901673866897921,
4.5709274611399));
#12532=CARTESIAN_POINT('Ctrl Pts',(-0.424576623578355,-2.31886419181245,
4.69789766839378));
#12533=CARTESIAN_POINT('Ctrl Pts',(1.71737702962559,-1.61493423626845,4.82486787564767));
#12534=CARTESIAN_POINT('Ctrl Pts',(2.28840502897144,0.566214511237573,4.95183808290156));
#12535=CARTESIAN_POINT('Ctrl Pts',(0.766174469238656,2.22943336568846,5.07880829015544));
#12536=CARTESIAN_POINT('Ctrl Pts',(-1.45689411749422,1.8533364453786,5.20577849740933));
#12537=CARTESIAN_POINT('Ctrl Pts',(-2.34730697130079,-0.218051443106043,
5.33274870466322));
#12538=CARTESIAN_POINT('Ctrl Pts',(-1.09058225712671,-2.08998248552431,
5.4597189119171));
#12539=CARTESIAN_POINT('Ctrl Pts',(1.16372401066593,-2.05015679311548,5.58668911917098));
#12540=CARTESIAN_POINT('Ctrl Pts',(2.35354422162328,-0.13500387483914,5.71365932642487));
#12541=CARTESIAN_POINT('Ctrl Pts',(1.39052150324245,1.903640301732,5.84062953367876));
#12542=CARTESIAN_POINT('Ctrl Pts',(-0.844444337704187,2.20097937515945,
5.96759974093265));
#12543=CARTESIAN_POINT('Ctrl Pts',(-2.30697683962809,0.485030216355141,
6.09456994818653));
#12544=CARTESIAN_POINT('Ctrl Pts',(-1.65926270513453,-1.67458762825586,
6.22154015544043));
#12545=CARTESIAN_POINT('Ctrl Pts',(0.506218527102226,-2.3024203031107,6.3485103626943));
#12546=CARTESIAN_POINT('Ctrl Pts',(2.20864962127088,-0.824174313976057,
6.4754805699482));
#12547=CARTESIAN_POINT('Ctrl Pts',(1.8907763264874,1.40796354091743,6.60245077720207));
#12548=CARTESIAN_POINT('Ctrl Pts',(-0.156635087036384,2.35220362614869,
6.72942098445597));
#12549=CARTESIAN_POINT('Ctrl Pts',(-2.06076865750355,1.14482705663735,6.85639119170984));
#12550=CARTESIAN_POINT('Ctrl Pts',(-2.07986807711532,-1.10975007598764,
6.98336139896374));
#12551=CARTESIAN_POINT('Ctrl Pts',(-0.1964626520611,-2.34921239476192,7.11033160621761));
#12552=CARTESIAN_POINT('Ctrl Pts',(1.86665183793563,-1.43979420935406,7.23730181347151));
#12553=CARTESIAN_POINT('Ctrl Pts',(2.22229545319173,0.786638015914119,7.36427202072539));
#12554=CARTESIAN_POINT('Ctrl Pts',(0.54515251217721,2.29351372087127,7.49124222797928));
#12555=CARTESIAN_POINT('Ctrl Pts',(-1.63065440993819,1.70245782464854,7.61821243523317));
#12556=CARTESIAN_POINT('Ctrl Pts',(-2.31486292299194,-0.445876773464548,
7.74518264248704));
#12557=CARTESIAN_POINT('Ctrl Pts',(-0.8816112114347,-2.18635727209223,7.87215284974095));
#12558=CARTESIAN_POINT('Ctrl Pts',(1.35807126336241,-1.92692472426588,7.99912305699481));
#12559=CARTESIAN_POINT('Ctrl Pts',(2.35549362254096,0.0951117423181714,
8.12609326424872));
#12560=CARTESIAN_POINT('Ctrl Pts',(1.19828988895336,2.03014723391927,8.25306347150259));
#12561=CARTESIAN_POINT('Ctrl Pts',(-1.05501813323409,2.10815871980864,8.38003367875648));
#12562=CARTESIAN_POINT('Ctrl Pts',(-2.34327595258744,0.257787236657217,
8.50700388601036));
#12563=CARTESIAN_POINT('Ctrl Pts',(-1.48808347274196,-1.8283883688949,8.63397409326426));
#12564=CARTESIAN_POINT('Ctrl Pts',(0.72829438578655,-2.24209360575996,8.76094430051814));
#12565=CARTESIAN_POINT('Ctrl Pts',(2.27848403144356,-0.604902444874099,
8.88791450777203));
#12566=CARTESIAN_POINT('Ctrl Pts',(1.74449009064557,1.58560738299156,9.01488471502591));
#12567=CARTESIAN_POINT('Ctrl Pts',(-0.385230466394427,2.32572438975891,
9.1418549222798));
#12568=CARTESIAN_POINT('Ctrl Pts',(-2.1625715448067,0.938445929689231,9.26882512953368));
#12569=CARTESIAN_POINT('Ctrl Pts',(-1.96175694776964,-1.30725136344754,
9.39579533678757));
#12570=CARTESIAN_POINT('Ctrl Pts',(0.0335234320998379,-2.35717471326548,
9.52276554404145));
#12571=CARTESIAN_POINT('Ctrl Pts',(1.99813913054961,-1.25093423661054,9.64973575129535));
#12572=CARTESIAN_POINT('Ctrl Pts',(2.13500939744307,0.999565566727712,9.77670595854921));
#12573=CARTESIAN_POINT('Ctrl Pts',(0.318935741240959,2.33573894995075,9.90367616580313));
#12574=CARTESIAN_POINT('Ctrl Pts',(-1.78887603024087,1.53535630971693,10.030646373057));
#12575=CARTESIAN_POINT('Ctrl Pts',(-2.26036030985581,-0.669453298585103,
10.1576165803109));
#12576=CARTESIAN_POINT('Ctrl Pts',(-0.664239202615746,-2.26189803728336,
10.2845867875648));
#12577=CARTESIAN_POINT('Ctrl Pts',(1.53947731651516,-1.78533079324062,10.4115569948187));
#12578=CARTESIAN_POINT('Ctrl Pts',(2.33499728455247,0.32432102998492,10.5385272020725));
#12579=CARTESIAN_POINT('Ctrl Pts',(0.994639648129273,2.13730868611139,10.6654974093264));
#12580=CARTESIAN_POINT('Ctrl Pts',(-1.25553855339793,1.9952492050592,10.7924676165803));
#12581=CARTESIAN_POINT('Ctrl Pts',(-2.35724575006339,0.028087776096,10.9194378238342));
#12582=CARTESIAN_POINT('Ctrl Pts',(-1.30272414120579,-1.96476621033587,
11.0464080310881));
#12583=CARTESIAN_POINT('Ctrl Pts',(0.943430253008483,-2.16040176982576,
11.173378238342));
#12584=CARTESIAN_POINT('Ctrl Pts',(2.32660653495589,-0.379866398696293,
11.3003484455959));
#12585=CARTESIAN_POINT('Ctrl Pts',(1.58158043085374,1.74814181063735,11.4273186528497));
#12586=CARTESIAN_POINT('Ctrl Pts',(-0.610154945358331,2.27708308851757,
11.5542888601037));
#12587=CARTESIAN_POINT('Ctrl Pts',(-2.24376706735364,0.723122255788841,
11.6812590673575));
#12588=CARTESIAN_POINT('Ctrl Pts',(-1.82495203643891,-1.4922957193718,11.8082292746114));
#12589=CARTESIAN_POINT('Ctrl Pts',(0.263190068058092,-2.34267527357795,
11.9351994818653));
#12590=CARTESIAN_POINT('Ctrl Pts',(2.11058595164912,-1.05015398397536,12.0621696891192));
#12591=CARTESIAN_POINT('Ctrl Pts',(2.0273786194508,1.20296815533566,12.1891398963731));
#12592=CARTESIAN_POINT('Ctrl Pts',(0.0896797991062791,2.35570668441345,
12.316110103627));
#12593=CARTESIAN_POINT('Ctrl Pts',(-1.93005126844934,1.35362422795805,12.4430803108808));
#12594=CARTESIAN_POINT('Ctrl Pts',(-2.18431849285034,-0.886650534962871,
12.5700505181347));
#12595=CARTESIAN_POINT('Ctrl Pts',(-0.440537590706227,-2.31588494544368,
12.6970207253886));
#12596=CARTESIAN_POINT('Ctrl Pts',(1.70621353334662,-1.62672426304606,12.8239909326425));
#12597=CARTESIAN_POINT('Ctrl Pts',(2.29225051935244,0.550439829487665,12.9509611398964));
#12598=CARTESIAN_POINT('Ctrl Pts',(0.781511384680127,2.22410350590373,13.0779313471503));
#12599=CARTESIAN_POINT('Ctrl Pts',(-1.44409481866595,1.86332675718997,13.2049015544042));
#12600=CARTESIAN_POINT('Ctrl Pts',(-2.34875311243137,-0.201879335747595,
13.331871761658));
#12601=CARTESIAN_POINT('Ctrl Pts',(-1.10495101849633,-2.08242159422195,
13.4588419689119));
#12602=CARTESIAN_POINT('Ctrl Pts',(1.14957607715301,-2.05812324514239,13.5858121761658));
#12603=CARTESIAN_POINT('Ctrl Pts',(2.35255856756512,-0.151210566872388,
13.7127823834197));
#12604=CARTESIAN_POINT('Ctrl Pts',(1.40359972987109,1.894018016721,13.8397525906736));
#12605=CARTESIAN_POINT('Ctrl Pts',(-0.829265195633706,2.20674323034388,
13.9667227979275));
#12606=CARTESIAN_POINT('Ctrl Pts',(-2.30358150473097,0.500907876180168,
14.0936930051813));
#12607=CARTESIAN_POINT('Ctrl Pts',(-1.67075697107245,-1.66311983722483,
14.2206632124353));
#12608=CARTESIAN_POINT('Ctrl Pts',(0.490348739021751,-2.30585224233855,
14.3476334196891));
#12609=CARTESIAN_POINT('Ctrl Pts',(2.20292078401032,-0.839366706948347,
14.474603626943));
#12610=CARTESIAN_POINT('Ctrl Pts',(1.90042874387294,1.39490753773124,14.6015738341969));
#12611=CARTESIAN_POINT('Ctrl Pts',(-0.140430710978244,2.35322664968167,
14.7285440414508));
#12612=CARTESIAN_POINT('Ctrl Pts',(-2.05283485132384,1.15899332290923,14.8555142487047));
#12613=CARTESIAN_POINT('Ctrl Pts',(-2.08746208220335,-1.095398787986,14.9824844559586));
#12614=CARTESIAN_POINT('Ctrl Pts',(-0.21263805117564,-2.34780354982058,
15.1094546632124));
#12615=CARTESIAN_POINT('Ctrl Pts',(1.85669106744545,-1.45261651148066,15.2364248704663));
#12616=CARTESIAN_POINT('Ctrl Pts',(2.22766066522509,0.771313431729834,15.3633950777202));
#12617=CARTESIAN_POINT('Ctrl Pts',(0.560936019559882,2.28970461660849,15.4903652849741));
#12618=CARTESIAN_POINT('Ctrl Pts',(-1.61889015716034,1.71364847865813,15.617335492228));
#12619=CARTESIAN_POINT('Ctrl Pts',(-2.31787896690132,-0.429922718816292,
15.7443056994818));
#12620=CARTESIAN_POINT('Ctrl Pts',(-0.896648704865739,-2.18023337040339,
15.8712759067358));
#12621=CARTESIAN_POINT('Ctrl Pts',(1.34476747364227,-1.93623265420035,15.9982461139896));
#12622=CARTESIAN_POINT('Ctrl Pts',(2.35609282970634,0.0788861658613507,
16.1252163212435));
#12623=CARTESIAN_POINT('Ctrl Pts',(1.21224398394502,2.02184593200051,16.2521865284974));
#12624=CARTESIAN_POINT('Ctrl Pts',(-1.04047329330418,2.11537509091856,16.3791567357513));
#12625=CARTESIAN_POINT('Ctrl Pts',(-2.34144487906595,0.273920294344516,
16.5061269430052));
#12626=CARTESIAN_POINT('Ctrl Pts',(-1.50064109217059,-1.81809591656959,
16.6330971502591));
#12627=CARTESIAN_POINT('Ctrl Pts',(0.712834826853045,-2.24705650996661,
16.760067357513));
#12628=CARTESIAN_POINT('Ctrl Pts',(2.27426375960074,-0.620581018985151,
16.8870375647669));
#12629=CARTESIAN_POINT('Ctrl Pts',(1.75536948901827,1.57355470396859,17.0140077720207));
#12630=CARTESIAN_POINT('Ctrl Pts',(-0.36920304249889,2.32832247825929,17.1409779792746));
#12631=CARTESIAN_POINT('Ctrl Pts',(-2.1560567615836,0.953318252310089,17.2679481865285));
#12632=CARTESIAN_POINT('Ctrl Pts',(-1.9707140325278,-1.29370887426652,17.3949183937824));
#12633=CARTESIAN_POINT('Ctrl Pts',(0.0172877380261932,-2.35734969477841,
17.5218886010363));
#12634=CARTESIAN_POINT('Ctrl Pts',(1.98947600304585,-1.26466662906185,17.6488588082902));
#12635=CARTESIAN_POINT('Ctrl Pts',(2.14184320547626,0.984837109634436,17.775829015544));
#12636=CARTESIAN_POINT('Ctrl Pts',(0.335015437913597,2.33348689855279,17.902799222798));
#12637=CARTESIAN_POINT('Ctrl Pts',(-1.7782589262777,1.54764066904162,18.0297694300518));
#12638=CARTESIAN_POINT('Ctrl Pts',(-2.26491751635406,-0.653869324460531,
18.1567396373057));
#12639=CARTESIAN_POINT('Ctrl Pts',(-0.679802134300005,-2.25726948049166,
18.2837098445596));
#12640=CARTESIAN_POINT('Ctrl Pts',(1.52714444375655,-1.79589150486922,18.4106800518135));
#12641=CARTESIAN_POINT('Ctrl Pts',(2.33717564303521,0.30823118427704,18.5376502590674));
#12642=CARTESIAN_POINT('Ctrl Pts',(1.00933664148997,2.13040747123729,18.6646204663213));
#12643=CARTESIAN_POINT('Ctrl Pts',(-1.24176661487133,2.00384932655849,18.7915906735751));
#12644=CARTESIAN_POINT('Ctrl Pts',(-2.35699638640381,0.0443224980938706,
18.918560880829));
#12645=CARTESIAN_POINT('Ctrl Pts',(-1.31622545128915,-1.95574717454394,
19.0455310880829));
#12646=CARTESIAN_POINT('Ctrl Pts',(0.928528238935361,-2.16684834699098,
19.1725012953368));
#12647=CARTESIAN_POINT('Ctrl Pts',(2.32393504393153,-0.395881751214744,
19.2994715025907));
#12648=CARTESIAN_POINT('Ctrl Pts',(1.59358313931722,1.73720730698498,19.4264417098446));
#12649=CARTESIAN_POINT('Ctrl Pts',(-0.594457200581991,2.28123148453506,
19.5534119170984));
#12650=CARTESIAN_POINT('Ctrl Pts',(-2.23873338712067,0.738558914880064,
19.6803821243523));
#12651=CARTESIAN_POINT('Ctrl Pts',(-1.83518684789343,-1.47969107677181,
19.8073523316062));
#12652=CARTESIAN_POINT('Ctrl Pts',(0.247048790610012,-2.34443241412816,
19.9343225388601));
#12653=CARTESIAN_POINT('Ctrl Pts',(2.10330301895634,-1.0646656093841,20.061292746114));
#12654=CARTESIAN_POINT('Ctrl Pts',(2.0356159034317,1.18897617430391,20.1882629533679));
#12655=CARTESIAN_POINT('Ctrl Pts',(0.10590245999703,2.35503314590555,20.3152331606218));
#12656=CARTESIAN_POINT('Ctrl Pts',(-1.92068248476191,1.36688523368939,20.4422033678757));
#12657=CARTESIAN_POINT('Ctrl Pts',(-2.1903734358619,-0.871585142648238,
20.5691735751295));
#12658=CARTESIAN_POINT('Ctrl Pts',(-0.456477659862079,-2.31279583952387,
20.6961437823834));
#12659=CARTESIAN_POINT('Ctrl Pts',(1.6949690987159,-1.63843712229916,20.8231139896373));
#12660=CARTESIAN_POINT('Ctrl Pts',(2.29598727142038,0.534639036362976,20.9500841968912));
#12661=CARTESIAN_POINT('Ctrl Pts',(0.796811227132131,2.21866814035183,21.0770544041451));
#12662=CARTESIAN_POINT('Ctrl Pts',(-1.43122701550266,1.87322867783953,21.204024611399));
#12663=CARTESIAN_POINT('Ctrl Pts',(-2.35008783531489,-0.185697652132911,
21.3309948186529));
#12664=CARTESIAN_POINT('Ctrl Pts',(-1.1192673629799,-2.07476191756569,21.4579650259067));
#12665=CARTESIAN_POINT('Ctrl Pts',(1.13537360904899,-2.06599206652615,21.5849352331606));
#12666=CARTESIAN_POINT('Ctrl Pts',(2.3514613175128,-0.167410083297791,21.7119054404145));
#12667=CARTESIAN_POINT('Ctrl Pts',(1.41661136721561,1.88430587953843,21.8388756476684));
#12668=CARTESIAN_POINT('Ctrl Pts',(-0.814046703622753,2.21240241272419,
21.9658458549223));
#12669=CARTESIAN_POINT('Ctrl Pts',(-2.30007691634645,0.516761756465324,
22.0928160621762));
#12670=CARTESIAN_POINT('Ctrl Pts',(-1.68217193798728,-1.65157311827105,
22.2197862694301));
#12671=CARTESIAN_POINT('Ctrl Pts',(0.474455608801953,-2.30917486244222,
22.3467564766839));
#12672=CARTESIAN_POINT('Ctrl Pts',(2.19708760073256,-0.854519159734979,
22.4737266839378));
#12673=CARTESIAN_POINT('Ctrl Pts',(1.90999071506285,1.3817851298529,22.6006968911917));
#12674=CARTESIAN_POINT('Ctrl Pts',(-0.124219111753841,2.35413848780229,
22.7276670984456));
#12675=CARTESIAN_POINT('Ctrl Pts',(-2.0448047334343,1.17310376104416,22.8546373056995));
#12676=CARTESIAN_POINT('Ctrl Pts',(-2.09495502675834,-1.08099392105983,
22.9816075129534));
#12677=CARTESIAN_POINT('Ctrl Pts',(-0.228807242491405,-2.34628640912002,
23.1085777202073));
#12678=CARTESIAN_POINT('Ctrl Pts',(1.84664960858395,-1.46536404316653,23.2355479274611));
#12679=CARTESIAN_POINT('Ctrl Pts',(2.23290613147693,0.755941093646845,23.3625181347151));
#12680=CARTESIAN_POINT('Ctrl Pts',(0.576719717599789,2.28580815893301,23.4894883419689));
#12681=CARTESIAN_POINT('Ctrl Pts',(-1.60710015146648,1.72471734220924,23.6164585492229));
#12682=CARTESIAN_POINT('Ctrl Pts',(-2.32068783736058,-0.413871133396448,
23.7434287564766));
#12683=CARTESIAN_POINT('Ctrl Pts',(-0.911828861708041,-2.17415297545205,
23.8703989637307));
#12684=CARTESIAN_POINT('Ctrl Pts',(1.33175293478252,-1.94516872322012,23.9973691709844));
#12685=CARTESIAN_POINT('Ctrl Pts',(2.35590509889789,0.0621220732712832,
24.1243393782384));
#12686=CARTESIAN_POINT('Ctrl Pts',(1.22745053520999,2.01448000455152,24.2513095854922));
#12687=CARTESIAN_POINT('Ctrl Pts',(-1.02858118383587,2.12041610541359,24.3782797927461));
#12688=CARTESIAN_POINT('Ctrl Pts',(-1.89801534866759,0.903452385056865,
24.4629265975821));
#12689=CARTESIAN_POINT('Ctrl Pts',(-1.97959496748082,0.245420714742313,
24.50525));
#12690=CARTESIAN_POINT('',(1.16034898466906,-1.62253437445173,0.));
#12691=CARTESIAN_POINT('Ctrl Pts',(1.160348984669,-1.62253437445178,0.));
#12692=CARTESIAN_POINT('Ctrl Pts',(1.69969113399867,-1.23682598810383,0.0423234024179621));
#12693=CARTESIAN_POINT('Ctrl Pts',(2.35424863102644,0.107968028363325,0.126970207253886));
#12694=CARTESIAN_POINT('Ctrl Pts',(1.18456011268651,2.03999555013175,0.253940414507772));
#12695=CARTESIAN_POINT('Ctrl Pts',(-1.06966068457706,2.09999381115058,0.380910621761658));
#12696=CARTESIAN_POINT('Ctrl Pts',(-1.9636032657455,0.797619232342793,0.469915444057474));
#12697=CARTESIAN_POINT('Ctrl Pts',(-1.99761127318624,0.0693315477139227,
0.516596863935328));
#12698=CARTESIAN_POINT('Ctrl Pts',(-1.99714087507904,0.00129381383500625,
0.52095488139522));
#12699=CARTESIAN_POINT('Ctrl Pts',(1.07765127757231,2.20530172674001,7.97972798949331E-17));
#12700=CARTESIAN_POINT('Ctrl Pts',(1.12809639271741,2.17510065728148,6.86960599404408E-17));
#12701=CARTESIAN_POINT('Ctrl Pts',(1.17730025765894,2.14300509491081,1.10309490283818E-16));
#12702=CARTESIAN_POINT('Ctrl Pts',(1.22514132390505,2.1090085670223,1.26634813746307E-16));
#12703=CARTESIAN_POINT('Ctrl Pts',(1.29462421705668,2.05963305555998,1.57121996985627E-16));
#12704=CARTESIAN_POINT('Ctrl Pts',(1.36123441505861,2.00624872602741,1.84001859055496E-16));
#12705=CARTESIAN_POINT('Ctrl Pts',(1.42480302814056,1.94921747509588,1.31838984174237E-16));
#12706=CARTESIAN_POINT('Ctrl Pts',(1.45690053415869,1.92042085941958,1.05500542776029E-16));
#12707=CARTESIAN_POINT('Ctrl Pts',(1.48822193239482,1.89069393167789,-1.71410280842816E-16));
#12708=CARTESIAN_POINT('Ctrl Pts',(1.51874122959272,1.86008072957315,-2.1163626406917E-16));
#12709=CARTESIAN_POINT('Ctrl Pts',(1.53250999529149,1.84626959872253,-2.29784196325102E-16));
#12710=CARTESIAN_POINT('Ctrl Pts',(1.54611546415791,1.83227806106527,-6.87915904046554E-17));
#12711=CARTESIAN_POINT('Ctrl Pts',(1.55955504465434,1.81811008308972,-8.32667268468867E-17));
#12712=CARTESIAN_POINT('Ctrl Pts',(1.57081510549093,1.80623975023383,-9.53944057577452E-17));
#12713=CARTESIAN_POINT('Ctrl Pts',(1.5819588119139,1.79424531325038,-9.69640209386679E-17));
#12714=CARTESIAN_POINT('Ctrl Pts',(1.59297464935461,1.7821404241451,-1.17961196366423E-16));
#12715=CARTESIAN_POINT('Ctrl Pts',(1.65014233615335,1.7193210050289,-2.26927941289128E-16));
#12716=CARTESIAN_POINT('Ctrl Pts',(1.70393951009346,1.65345682333213,-6.05899575447923E-16));
#12717=CARTESIAN_POINT('Ctrl Pts',(1.75419867452451,1.58490693773027,-5.20417042793042E-16));
#12718=CARTESIAN_POINT('Ctrl Pts',(1.79330135022385,1.53157370037424,-4.53909853702211E-16));
#12719=CARTESIAN_POINT('Ctrl Pts',(1.83026160943548,1.47661394117244,-5.4299838061594E-16));
#12720=CARTESIAN_POINT('Ctrl Pts',(1.86498033301496,1.42018860836785,-6.45317133063372E-16));
#12721=CARTESIAN_POINT('Ctrl Pts',(1.88104710033835,1.39407668373901,-6.92667133838316E-16));
#12722=CARTESIAN_POINT('Ctrl Pts',(1.89663356986419,1.3676508303538,-1.30333522663486E-16));
#12723=CARTESIAN_POINT('Ctrl Pts',(1.91172852635572,1.34092677154389,-1.52655665885959E-16));
#12724=CARTESIAN_POINT('Ctrl Pts',(1.9192190540249,1.32766556724293,-1.63732520035034E-16));
#12725=CARTESIAN_POINT('Ctrl Pts',(1.92658853680698,1.31433093124829,-4.1258915407781E-16));
#12726=CARTESIAN_POINT('Ctrl Pts',(1.93383552001789,1.30092478157845,-4.30211422042248E-16));
#12727=CARTESIAN_POINT('Ctrl Pts',(1.9407073591395,1.28821260865211,-4.46921463570597E-16));
#12728=CARTESIAN_POINT('Ctrl Pts',(1.94746478045741,1.27544399500121,-6.09762297626216E-16));
#12729=CARTESIAN_POINT('Ctrl Pts',(1.95410541003034,1.26262383458428,-5.82867087928207E-16));
#12730=CARTESIAN_POINT('Ctrl Pts',(1.99234448003475,1.18880086248997,-4.27995054315904E-16));
#12731=CARTESIAN_POINT('Ctrl Pts',(2.0267328516625,1.11323685926757,-3.04131430563134E-16));
#12732=CARTESIAN_POINT('Ctrl Pts',(2.05710895345793,1.03626323191291,-2.77555756156289E-16));
#12733=CARTESIAN_POINT('Ctrl Pts',(2.08682191459507,0.960970015766318,-2.51560255279913E-16));
#12734=CARTESIAN_POINT('Ctrl Pts',(2.11269600419783,0.884327115080494,-2.74271135208625E-16));
#12735=CARTESIAN_POINT('Ctrl Pts',(2.13453193486002,0.806636355014066,-4.02455846426619E-16));
#12736=CARTESIAN_POINT('Ctrl Pts',(2.15588460824072,0.730664991573634,-5.27803664817409E-16));
#12737=CARTESIAN_POINT('Ctrl Pts',(2.17337597523708,0.65369086607791,1.83917474183848E-16));
#12738=CARTESIAN_POINT('Ctrl Pts',(2.18677163924531,0.576000526431045,1.80411241501588E-16));
#12739=CARTESIAN_POINT('Ctrl Pts',(2.19271177554795,0.541549736487604,1.78856447351139E-16));
#12740=CARTESIAN_POINT('Ctrl Pts',(2.19784589713018,0.506958238696871,2.58667507258439E-16));
#12741=CARTESIAN_POINT('Ctrl Pts',(2.20215036681449,0.472251887192273,3.05311331771918E-16));
#12742=CARTESIAN_POINT('Ctrl Pts',(2.20384086463367,0.45862163402915,3.23629798250044E-16));
#12743=CARTESIAN_POINT('Ctrl Pts',(2.2054034189863,0.444972429750506,-2.67189007756782E-16));
#12744=CARTESIAN_POINT('Ctrl Pts',(2.20683493494602,0.431323439258898,-2.63677968348475E-16));
#12745=CARTESIAN_POINT('Ctrl Pts',(2.21498668224708,0.353599456758773,-2.43684404304575E-16));
#12746=CARTESIAN_POINT('Ctrl Pts',(2.21891062752072,0.275752097207065,-3.64361181543216E-16));
#12747=CARTESIAN_POINT('Ctrl Pts',(2.21842976595528,0.198061284129886,-3.33066907387547E-16));
#12748=CARTESIAN_POINT('Ctrl Pts',(2.21823573988328,0.166713294655633,-3.2043976991813E-16));
#12749=CARTESIAN_POINT('Ctrl Pts',(2.21732398879068,0.135390827244206,1.47149945777791E-16));
#12750=CARTESIAN_POINT('Ctrl Pts',(2.2156804758574,0.104112597082251,1.11022302462516E-16));
#12751=CARTESIAN_POINT('Ctrl Pts',(2.21152549973649,0.0250378926516813,
4.83300826707103E-17));
#12752=CARTESIAN_POINT('Ctrl Pts',(2.20269687630619,-0.0537556215354904,
1.12975204580772E-16));
#12753=CARTESIAN_POINT('Ctrl Pts',(2.18938140457229,-0.131948941326607,
2.22044604925031E-16));
#12754=CARTESIAN_POINT('Ctrl Pts',(2.17635609001487,-0.208438352060393,
3.28737276162242E-16));
#12755=CARTESIAN_POINT('Ctrl Pts',(2.15903660233486,-0.284354146944832,
-3.46781305756475E-18));
#12756=CARTESIAN_POINT('Ctrl Pts',(2.13755823881172,-0.359371484419528,
-2.77555756156289E-17));
#12757=CARTESIAN_POINT('Ctrl Pts',(2.1327132344274,-0.376293599019833,-3.32343131345551E-17));
#12758=CARTESIAN_POINT('Ctrl Pts',(2.12765471739374,-0.393175045967983,
4.78722657737561E-16));
#12759=CARTESIAN_POINT('Ctrl Pts',(2.12239384145498,-0.409981702546287,
4.44089209850063E-16));
#12760=CARTESIAN_POINT('Ctrl Pts',(2.09915475041265,-0.484222461478205,
2.91101407450622E-16));
#12761=CARTESIAN_POINT('Ctrl Pts',(2.07194581573642,-0.557102807454745,
-2.6612583612487E-16));
#12762=CARTESIAN_POINT('Ctrl Pts',(2.04097168255273,-0.628331757793453,
-2.22044604925031E-16));
#12763=CARTESIAN_POINT('Ctrl Pts',(2.01002093348238,-0.699506933395764,
-1.77996653123198E-16));
#12764=CARTESIAN_POINT('Ctrl Pts',(1.97530999561803,-0.769034032577632,
-1.121614477549E-16));
#12765=CARTESIAN_POINT('Ctrl Pts',(1.93700033421706,-0.836593525678529,
2.77555756156289E-17));
#12766=CARTESIAN_POINT('Ctrl Pts',(1.89932999797199,-0.903025562104548,
1.65337614298032E-16));
#12767=CARTESIAN_POINT('Ctrl Pts',(1.85817935571419,-0.967555768065582,
3.22342438988347E-17));
#12768=CARTESIAN_POINT('Ctrl Pts',(1.81367086799685,-1.02984130765996,-8.32667268468867E-17));
#12769=CARTESIAN_POINT('Ctrl Pts',(1.79658036652,-1.05375789438347,-1.27617133080496E-16));
#12770=CARTESIAN_POINT('Ctrl Pts',(1.77899449903844,-1.07734305613259,3.71946656281201E-16));
#12771=CARTESIAN_POINT('Ctrl Pts',(1.76091927483634,-1.10057551065294,3.88578058618805E-16));
#12772=CARTESIAN_POINT('Ctrl Pts',(1.75330082146927,-1.11036766423216,3.955879613299E-16));
#12773=CARTESIAN_POINT('Ctrl Pts',(1.74559525034806,-1.120097236073,1.9277708950897E-16));
#12774=CARTESIAN_POINT('Ctrl Pts',(1.73781239012482,-1.12975130031544,1.94289029309402E-16));
#12775=CARTESIAN_POINT('Ctrl Pts',(1.69074076256592,-1.18814018350429,2.03433413910443E-16));
#12776=CARTESIAN_POINT('Ctrl Pts',(1.64076328117284,-1.24387604119422,4.01743023928347E-16));
#12777=CARTESIAN_POINT('Ctrl Pts',(1.58803301465667,-1.29667365960222,3.05311331771918E-16));
#12778=CARTESIAN_POINT('Ctrl Pts',(1.53615694857719,-1.34861598651105,2.10441778383092E-16));
#12779=CARTESIAN_POINT('Ctrl Pts',(1.48161590224946,-1.39771505374416,-1.45218570660009E-16));
#12780=CARTESIAN_POINT('Ctrl Pts',(1.42452885193311,-1.44365737342775,-1.94289029309402E-16));
#12781=CARTESIAN_POINT('Ctrl Pts',(1.36926934746984,-1.48812892705576,-2.4178857979808E-16));
#12782=CARTESIAN_POINT('Ctrl Pts',(1.31162365747817,-1.52964292911451,3.44150135834905E-16));
#12783=CARTESIAN_POINT('Ctrl Pts',(1.2516834907043,-1.56786936325681,3.33066907387547E-16));
#12784=CARTESIAN_POINT('Ctrl Pts',(1.22180547848687,-1.58692386256512,3.27542317571039E-16));
#12785=CARTESIAN_POINT('Ctrl Pts',(1.19135716333746,-1.60516076076372,2.09022357500404E-16));
#12786=CARTESIAN_POINT('Ctrl Pts',(1.160348984669,-1.62253437445177,2.22044604925031E-16));
#12787=CARTESIAN_POINT('Ctrl Pts',(0.159495341662761,2.44078487595691,24.0495));
#12788=CARTESIAN_POINT('Ctrl Pts',(0.553879590005283,2.41556185851724,24.0290607334364));
#12789=CARTESIAN_POINT('Ctrl Pts',(0.942374040131692,2.30021073164513,24.0086214668727));
#12790=CARTESIAN_POINT('Ctrl Pts',(1.27702530809929,2.09669071408131,23.9881822003091));
#12791=CARTESIAN_POINT('Ctrl Pts',(1.96998462930408,1.67526367428817,23.9458587978911));
#12792=CARTESIAN_POINT('Ctrl Pts',(2.43207727388235,0.875789536242101,23.9035353954731));
#12793=CARTESIAN_POINT('Ctrl Pts',(2.45343275118969,0.0650681252545471,
23.8612119930552));
#12794=CARTESIAN_POINT('Ctrl Pts',(2.47478822849703,-0.745653285733007,
23.8188885906372));
#12795=CARTESIAN_POINT('Ctrl Pts',(2.05540653853344,-1.56762196966205,23.7765651882193));
#12796=CARTESIAN_POINT('Ctrl Pts',(1.38635176387791,-2.02548987348432,23.7342417858013));
#12797=CARTESIAN_POINT('Ctrl Pts',(0.717296989222389,-2.48335777730658,
23.6919183833833));
#12798=CARTESIAN_POINT('Ctrl Pts',(-0.201430870125064,-2.57712490102209,
23.6495949809654));
#12799=CARTESIAN_POINT('Ctrl Pts',(-0.94925274522526,-2.26359816468399,
23.6072715785474));
#12800=CARTESIAN_POINT('Ctrl Pts',(-1.69707462032548,-1.95007142834589,
23.5649481761294));
#12801=CARTESIAN_POINT('Ctrl Pts',(-2.27399051117843,-1.22925083195416,
23.5226247737115));
#12802=CARTESIAN_POINT('Ctrl Pts',(-2.41634438138384,-0.430973544622496,
23.4803013712935));
#12803=CARTESIAN_POINT('Ctrl Pts',(-2.44154118278753,-0.289677531771226,
23.4728100795997));
#12804=CARTESIAN_POINT('Ctrl Pts',(-2.4531234108498,-0.145954846202415,
23.4653187879059));
#12805=CARTESIAN_POINT('Ctrl Pts',(-2.45183158050284,-0.00202607996204418,
23.457827496212));
#12806=CARTESIAN_POINT('Origin',(0.,0.,-1.47904511860479));
#12807=CARTESIAN_POINT('',(-1.16034898466913,-1.62253437445168,0.));
#12808=CARTESIAN_POINT('Ctrl Pts',(-1.16284465745828,-1.62479335886122,
1.03432887255117E-15));
#12809=CARTESIAN_POINT('Ctrl Pts',(-0.662089630281565,-1.97916236613021,
0.0393081915296248));
#12810=CARTESIAN_POINT('Ctrl Pts',(0.746426826565863,-2.20908649969502,
0.120955489700587));
#12811=CARTESIAN_POINT('Ctrl Pts',(2.27348886028002,-0.624404468413451,
0.244941894512889));
#12812=CARTESIAN_POINT('Ctrl Pts',(1.75738237739457,1.57205987855945,0.371959214436904));
#12813=CARTESIAN_POINT('Ctrl Pts',(-0.367613798684614,2.32876162996938,
0.498976534360922));
#12814=CARTESIAN_POINT('Ctrl Pts',(-1.80883238148956,1.22105962818686,0.601338502416877));
#12815=CARTESIAN_POINT('Ctrl Pts',(-1.99291933052672,0.27887251148749,0.661361363831493));
#12816=CARTESIAN_POINT('Ctrl Pts',(-1.99183435874083,0.00088002408572329,
0.679045118604771));
#12817=CARTESIAN_POINT('Origin',(0.,0.,0.));
#12818=CARTESIAN_POINT('Ctrl Pts',(-0.875140871775308,1.79252782880723,
-0.263127385183177));
#12819=CARTESIAN_POINT('Ctrl Pts',(-1.47121116518756,1.50151673942109,-0.220788278541838));
#12820=CARTESIAN_POINT('Ctrl Pts',(-2.33993822790823,0.283206897790784,
-0.13611006525916));
#12821=CARTESIAN_POINT('Ctrl Pts',(-1.50537684452792,-1.81659298312073,
-0.00909274533514401));
#12822=CARTESIAN_POINT('Ctrl Pts',(0.709096964461084,-2.24782491398444,
0.117924574588872));
#12823=CARTESIAN_POINT('Ctrl Pts',(2.27348886028002,-0.624404468413451,
0.244941894512889));
#12824=CARTESIAN_POINT('Ctrl Pts',(1.75738237739457,1.57205987855945,0.371959214436904));
#12825=CARTESIAN_POINT('Ctrl Pts',(-0.367613798684614,2.32876162996938,
0.498976534360922));
#12826=CARTESIAN_POINT('Ctrl Pts',(-2.15597060042669,0.954253673420782,
0.625993854284938));
#12827=CARTESIAN_POINT('Ctrl Pts',(-1.97094594256774,-1.29394223767452,
0.753011174208954));
#12828=CARTESIAN_POINT('Ctrl Pts',(0.0182153715595747,-2.3576204698764,
0.88002849413297));
#12829=CARTESIAN_POINT('Ctrl Pts',(1.9906822371454,-1.26332101110348,1.00704581405699));
#12830=CARTESIAN_POINT('Ctrl Pts',(2.14099816144828,0.987384922727256,1.134063133981));
#12831=CARTESIAN_POINT('Ctrl Pts',(0.331555254300241,2.33427609427238,1.26108045390502));
#12832=CARTESIAN_POINT('Ctrl Pts',(-1.78137220841604,1.54450678564102,1.38809777382904));
#12833=CARTESIAN_POINT('Ctrl Pts',(-2.26373025095555,-0.659024375424702,
1.51511509375305));
#12834=CARTESIAN_POINT('Ctrl Pts',(-0.673992169187479,-2.25931816777247,
1.64213241367707));
#12835=CARTESIAN_POINT('Ctrl Pts',(1.53268116536722,-1.79155650545778,1.76914973360108));
#12836=CARTESIAN_POINT('Ctrl Pts',(2.33642193463667,0.316098985050819,1.8961670535251));
#12837=CARTESIAN_POINT('Ctrl Pts',(1.00152929412067,2.13441435022671,2.02318437344912));
#12838=CARTESIAN_POINT('Ctrl Pts',(-1.25010860812744,1.99900333994266,2.15020169337313));
#12839=CARTESIAN_POINT('Ctrl Pts',(-2.35746526350733,0.0338135367837335,
2.27721901329715));
#12840=CARTESIAN_POINT('Ctrl Pts',(-1.30692669699531,-1.96232728509918,
2.40423633322116));
#12841=CARTESIAN_POINT('Ctrl Pts',(0.939901322271841,-2.16226069656491,
2.53125365314518));
#12842=CARTESIAN_POINT('Ctrl Pts',(2.32639490702415,-0.382978510636179,
2.6582709730692));
#12843=CARTESIAN_POINT('Ctrl Pts',(1.58343339573353,1.74686132178264,2.78528829299322));
#12844=CARTESIAN_POINT('Ctrl Pts',(-0.608916736747748,2.27771951988605,
2.91230561291723));
#12845=CARTESIAN_POINT('Ctrl Pts',(-2.24389767923029,0.723677418756311,
3.03932293284125));
#12846=CARTESIAN_POINT('Ctrl Pts',(-1.82493699351161,-1.49277954510288,
3.16634025276526));
#12847=CARTESIAN_POINT('Ctrl Pts',(0.264471544354857,-2.34282748059378,
3.29335757268928));
#12848=CARTESIAN_POINT('Ctrl Pts',(2.11179724612446,-1.04837884014621,3.42037489261329));
#12849=CARTESIAN_POINT('Ctrl Pts',(2.02609885609852,1.2056986466197,3.54739221253732));
#12850=CARTESIAN_POINT('Ctrl Pts',(0.0858200094412126,2.35614531115273,
3.67440953246132));
#12851=CARTESIAN_POINT('Ctrl Pts',(-1.93301379609718,1.34990498381208,3.80142685238535));
#12852=CARTESIAN_POINT('Ctrl Pts',(-2.1824721351227,-0.891964786655331,
3.92844417230936));
#12853=CARTESIAN_POINT('Ctrl Pts',(-0.434214441284883,-2.31737860959731,
4.05546149223338));
#12854=CARTESIAN_POINT('Ctrl Pts',(1.71149948445725,-1.62159036625522,4.18247881215739));
#12855=CARTESIAN_POINT('Ctrl Pts',(2.29060007052677,0.558513310613506,4.30949613208142));
#12856=CARTESIAN_POINT('Ctrl Pts',(0.77301020537091,2.22738434573485,4.43651345200542));
#12857=CARTESIAN_POINT('Ctrl Pts',(-1.4521510674508,1.85742915841551,4.56353077192945));
#12858=CARTESIAN_POINT('Ctrl Pts',(-2.34809240527012,-0.212715437953238,
4.69054809185345));
#12859=CARTESIAN_POINT('Ctrl Pts',(-1.09471794236404,-2.08815191686271,
4.81756541177748));
#12860=CARTESIAN_POINT('Ctrl Pts',(1.16070165538423,-2.05220794960434,4.94458273170149));
#12861=CARTESIAN_POINT('Ctrl Pts',(2.35367822395426,-0.13778468461515,5.07160005162551));
#12862=CARTESIAN_POINT('Ctrl Pts',(1.3922260378406,1.90275917046527,5.19861737154953));
#12863=CARTESIAN_POINT('Ctrl Pts',(-0.843593977493136,2.20162099426043,
5.32563469147353));
#12864=CARTESIAN_POINT('Ctrl Pts',(-2.30723404745788,0.485238963277019,
5.45265201139756));
#12865=CARTESIAN_POINT('Ctrl Pts',(-1.65895783037916,-1.67530436585556,
5.57966933132157));
#12866=CARTESIAN_POINT('Ctrl Pts',(0.507837960106644,-2.30236539400368,
5.70668665124559));
#12867=CARTESIAN_POINT('Ctrl Pts',(2.20978656254498,-0.821966635105482,
5.83370397116961));
#12868=CARTESIAN_POINT('Ctrl Pts',(1.88901699407625,1.41081557877779,5.96072129109363));
#12869=CARTESIAN_POINT('Ctrl Pts',(-0.160855766453599,2.35221411092393,
6.08773861101763));
#12870=CARTESIAN_POINT('Ctrl Pts',(-2.06348992610873,1.14052405765016,6.21475593094166));
#12871=CARTESIAN_POINT('Ctrl Pts',(-2.07731788168555,-1.11513955165281,
6.34177325086566));
#12872=CARTESIAN_POINT('Ctrl Pts',(-0.189682276366992,-2.35006519808776,
6.46879057078969));
#12873=CARTESIAN_POINT('Ctrl Pts',(1.87157814575952,-1.43386925678263,6.5958078907137));
#12874=CARTESIAN_POINT('Ctrl Pts',(2.21969794703782,0.794812446522514,6.72282521063772));
#12875=CARTESIAN_POINT('Ctrl Pts',(0.536027236282382,2.29596615898285,6.84984253056173));
#12876=CARTESIAN_POINT('Ctrl Pts',(-1.63829358942387,1.69551759533295,6.97685985048576));
#12877=CARTESIAN_POINT('Ctrl Pts',(-2.31300976155138,-0.456915357806061,
7.10387717040976));
#12878=CARTESIAN_POINT('Ctrl Pts',(-0.870522872770069,-2.19111289741426,
7.23089449033379));
#12879=CARTESIAN_POINT('Ctrl Pts',(1.3687932043082,-1.91968512133389,7.3579118102578));
#12880=CARTESIAN_POINT('Ctrl Pts',(2.35519059073263,0.108917778877055,7.48492913018183));
#12881=CARTESIAN_POINT('Ctrl Pts',(1.18577488435873,2.03782328106611,7.61194645010582));
#12882=CARTESIAN_POINT('Ctrl Pts',(-1.06903451833457,2.10141642704157,7.73896377002986));
#12883=CARTESIAN_POINT('Ctrl Pts',(-2.34530799262043,0.241487517237905,
7.86598108995386));
#12884=CARTESIAN_POINT('Ctrl Pts',(-1.47481436575085,-1.8394859031278,7.99299840987789));
#12885=CARTESIAN_POINT('Ctrl Pts',(0.745643944080418,-2.23669419230417,
8.1200157298019));
#12886=CARTESIAN_POINT('Ctrl Pts',(2.28358043018348,-0.586554532941333,
8.24703304972591));
#12887=CARTESIAN_POINT('Ctrl Pts',(1.73125186121253,1.60048517465147,8.37405036964994));
#12888=CARTESIAN_POINT('Ctrl Pts',(-0.405770296472382,2.32252799073159,
8.50106768957393));
#12889=CARTESIAN_POINT('Ctrl Pts',(-2.1713724420165,0.918655277719749,8.62808500949798));
#12890=CARTESIAN_POINT('Ctrl Pts',(-1.94941860875359,-1.32610440353548,
8.75510232942198));
#12891=CARTESIAN_POINT('Ctrl Pts',(0.0569267623458949,-2.35702039553327,
8.882119649346));
#12892=CARTESIAN_POINT('Ctrl Pts',(2.01116447809095,-1.23044839115509,9.00913696927002));
#12893=CARTESIAN_POINT('Ctrl Pts',(2.12449185277921,1.02240900265292,9.13615428919402));
#12894=CARTESIAN_POINT('Ctrl Pts',(0.293175184736282,2.33940892369971,9.26317160911806));
#12895=CARTESIAN_POINT('Ctrl Pts',(-1.80649806736613,1.51504142974158,9.39018892904205));
#12896=CARTESIAN_POINT('Ctrl Pts',(-2.25260145507328,-0.696112408905862,
9.51720624896608));
#12897=CARTESIAN_POINT('Ctrl Pts',(-0.636796252956758,-2.27008289131724,
9.64422356889009));
#12898=CARTESIAN_POINT('Ctrl Pts',(1.5618975293753,-1.76614323002478,9.77124088881411));
#12899=CARTESIAN_POINT('Ctrl Pts',(2.33091544739048,0.354427677174692,9.89825820873813));
#12900=CARTESIAN_POINT('Ctrl Pts',(0.966340415661779,2.15057480741536,10.0252755286621));
#12901=CARTESIAN_POINT('Ctrl Pts',(-1.28276996041703,1.97820297994991,10.1522928485862));
#12902=CARTESIAN_POINT('Ctrl Pts',(-2.35770263444618,-0.0049080298005949,
10.2793101685102));
#12903=CARTESIAN_POINT('Ctrl Pts',(-1.27452282778516,-1.98352649659275,
10.4063274884342));
#12904=CARTESIAN_POINT('Ctrl Pts',(0.975285705239301,-2.14653292413298,
10.5333448083582));
#12905=CARTESIAN_POINT('Ctrl Pts',(2.33237086341372,-0.344720113613569,
10.6603621282822));
#12906=CARTESIAN_POINT('Ctrl Pts',(1.5545308633467,1.77263069930924,10.7873794482062));
#12907=CARTESIAN_POINT('Ctrl Pts',(-0.646241956488163,2.2674119905534,10.9143967681303));
#12908=CARTESIAN_POINT('Ctrl Pts',(-2.25548011395016,0.686727935070636,
11.0414140880543));
#12909=CARTESIAN_POINT('Ctrl Pts',(-1.80017471415913,-1.52254944081731,
11.1684314079783));
#12910=CARTESIAN_POINT('Ctrl Pts',(0.302912497167387,-2.33816804791504,
11.2954487279023));
#12911=CARTESIAN_POINT('Ctrl Pts',(2.12873011938496,-1.01355507006492,11.4224660478263));
#12912=CARTESIAN_POINT('Ctrl Pts',(2.00602422063487,1.2388109732551,11.5494833677503));
#12913=CARTESIAN_POINT('Ctrl Pts',(0.0471130923241888,2.35723697530873,
11.6765006876744));
#12914=CARTESIAN_POINT('Ctrl Pts',(-1.95492279271505,1.31797673566501,11.8035180075984));
#12915=CARTESIAN_POINT('Ctrl Pts',(-2.16752890993496,-0.927687569080867,
11.9305353275224));
#12916=CARTESIAN_POINT('Ctrl Pts',(-0.396097208116597,-2.32419723839291,
12.0575526474464));
#12917=CARTESIAN_POINT('Ctrl Pts',(1.737900288011,-1.59326344028923,12.1845699673704));
#12918=CARTESIAN_POINT('Ctrl Pts',(2.28111858791796,0.596056867325744,12.3115872872944));
#12919=CARTESIAN_POINT('Ctrl Pts',(0.736325268973554,2.23977920775732,12.4386046072184));
#12920=CARTESIAN_POINT('Ctrl Pts',(-1.48246006643762,1.83332974465828,12.5656219271425));
#12921=CARTESIAN_POINT('Ctrl Pts',(-2.34428226122129,-0.251249837719779,
12.6926392470665));
#12922=CARTESIAN_POINT('Ctrl Pts',(-1.06027625346291,-2.10584901347975,
12.8196565669905));
#12923=CARTESIAN_POINT('Ctrl Pts',(1.19424884442458,-2.03286878544129,12.9466738869145));
#12924=CARTESIAN_POINT('Ctrl Pts',(2.35562364483704,-0.0991112764303932,
13.0736912068385));
#12925=CARTESIAN_POINT('Ctrl Pts',(1.36078895832842,1.92536729278402,13.2007085267625));
#12926=CARTESIAN_POINT('Ctrl Pts',(-0.879637768350177,2.18746958783955,
13.3277258466866));
#12927=CARTESIAN_POINT('Ctrl Pts',(-2.31489202814179,0.447281454205958,
13.4547431666106));
#12928=CARTESIAN_POINT('Ctrl Pts',(-1.6312203027841,-1.70232374271639,13.5817604865346));
#12929=CARTESIAN_POINT('Ctrl Pts',(0.545581575104675,-2.2937145738163,13.7087778064586));
#12930=CARTESIAN_POINT('Ctrl Pts',(2.22298781706136,-0.785564107140691,
13.8357951263826));
#12931=CARTESIAN_POINT('Ctrl Pts',(1.86559217928514,1.44164892460722,13.9628124463066));
#12932=CARTESIAN_POINT('Ctrl Pts',(-0.199464851904689,2.34925511047346,
14.0898297662307));
#12933=CARTESIAN_POINT('Ctrl Pts',(-2.08194262985648,1.10648121864643,14.2168470861547));
#12934=CARTESIAN_POINT('Ctrl Pts',(-2.05872360451754,-1.1491052699528,14.3438644060787));
#12935=CARTESIAN_POINT('Ctrl Pts',(-0.151061206087832,-2.35286342851562,
14.4708817260027));
#12936=CARTESIAN_POINT('Ctrl Pts',(1.89487438652815,-1.40293865172736,14.5978990459267));
#12937=CARTESIAN_POINT('Ctrl Pts',(2.2063452493004,0.831159697122361,14.7249163658507));
#12938=CARTESIAN_POINT('Ctrl Pts',(0.498247931734623,2.30445976310136,14.8519336857748));
#12939=CARTESIAN_POINT('Ctrl Pts',(-1.66591838462884,1.66838297071943,14.9789510056988));
#12940=CARTESIAN_POINT('Ctrl Pts',(-2.30519381562279,-0.494840654802578,
15.1059683256228));
#12941=CARTESIAN_POINT('Ctrl Pts',(-0.834420476588558,-2.20511411711067,
15.2329856455468));
#12942=CARTESIAN_POINT('Ctrl Pts',(1.40013588510504,-1.89694631038207,15.3600029654708));
#12943=CARTESIAN_POINT('Ctrl Pts',(2.35308417453332,0.147582752352149,15.4870202853949));
#12944=CARTESIAN_POINT('Ctrl Pts',(1.15214746973809,2.05702260785027,15.6140376053188));
#12945=CARTESIAN_POINT('Ctrl Pts',(-1.10340222895637,2.08357608989091,15.7410549252429));
#12946=CARTESIAN_POINT('Ctrl Pts',(-2.34895767021494,0.202937588360042,
15.8680722451669));
#12947=CARTESIAN_POINT('Ctrl Pts',(-1.44440529438039,-1.86345892007226,
15.9950895650909));
#12948=CARTESIAN_POINT('Ctrl Pts',(0.782276957985213,-2.22414670429727,
16.1221068850149));
#12949=CARTESIAN_POINT('Ctrl Pts',(2.2929055224434,-0.548971826580871,16.249124204939));
#12950=CARTESIAN_POINT('Ctrl Pts',(1.704733350654,1.62870193847707,16.3761415248629));
#12951=CARTESIAN_POINT('Ctrl Pts',(-0.443858810723858,2.31555072442255,
16.503158844787));
#12952=CARTESIAN_POINT('Ctrl Pts',(-2.18616681009904,0.882870590546761,
16.630176164711));
#12953=CARTESIAN_POINT('Ctrl Pts',(-1.92737687251849,-1.3579411594439,16.757193484635));
#12954=CARTESIAN_POINT('Ctrl Pts',(0.0956287989740662,-2.355767589139,16.884210804559));
#12955=CARTESIAN_POINT('Ctrl Pts',(2.03110108030785,-1.19725277314494,17.011228124483));
#12956=CARTESIAN_POINT('Ctrl Pts',(2.10741414159636,1.05716197294014,17.138245444407));
#12957=CARTESIAN_POINT('Ctrl Pts',(0.254715166118652,2.34390827153712,17.2652627643311));
#12958=CARTESIAN_POINT('Ctrl Pts',(-1.83113618870942,1.48516869736397,17.3922800842551));
#12959=CARTESIAN_POINT('Ctrl Pts',(-2.2408652858103,-0.733013350547816,
17.5192974041791));
#12960=CARTESIAN_POINT('Ctrl Pts',(-0.599428442729515,-2.28023493159759,
17.6463147241031));
#12961=CARTESIAN_POINT('Ctrl Pts',(1.5906925238854,-1.74025374462637,17.7733320440271));
#12962=CARTESIAN_POINT('Ctrl Pts',(2.32478025773261,0.392660864471763,17.9003493639512));
#12963=CARTESIAN_POINT('Ctrl Pts',(0.930890860039063,2.16615512092895,18.0273666838751));
#12964=CARTESIAN_POINT('Ctrl Pts',(-1.31508529103024,1.95686904992309,18.1543840037992));
#12965=CARTESIAN_POINT('Ctrl Pts',(-2.35730404781258,-0.0436282866660298,
18.2814013237232));
#12966=CARTESIAN_POINT('Ctrl Pts',(-1.24177516838345,-2.00419066768041,
18.4084186436472));
#12967=CARTESIAN_POINT('Ctrl Pts',(1.01040701496368,-2.13022615356754,18.5354359635712));
#12968=CARTESIAN_POINT('Ctrl Pts',(2.33771769089012,-0.306368730340369,
18.6624532834953));
#12969=CARTESIAN_POINT('Ctrl Pts',(1.52520901414179,1.79792192945402,18.7894706034193));
#12970=CARTESIAN_POINT('Ctrl Pts',(-0.683392859853091,2.25649285403983,
18.9164879233433));
#12971=CARTESIAN_POINT('Ctrl Pts',(-2.26645415951258,0.649593214295779,
19.0435052432673));
#12972=CARTESIAN_POINT('Ctrl Pts',(-1.77492685877157,-1.55190864655181,
19.1705225631913));
#12973=CARTESIAN_POINT('Ctrl Pts',(0.341271742863524,-2.33287792195687,
19.2975398831153));
#12974=CARTESIAN_POINT('Ctrl Pts',(2.14508879272012,-0.978457905368288,
19.4245572030393));
#12975=CARTESIAN_POINT('Ctrl Pts',(1.98540848369728,1.27158914516195,19.5515745229634));
#12976=CARTESIAN_POINT('Ctrl Pts',(0.00839346700838828,2.35769280249617,
19.6785918428874));
#12977=CARTESIAN_POINT('Ctrl Pts',(-1.97630447187918,1.2856929787716,19.8056091628114));
#12978=CARTESIAN_POINT('Ctrl Pts',(-2.15200101928721,-0.963160118680454,
19.9326264827354));
#12979=CARTESIAN_POINT('Ctrl Pts',(-0.357873132381371,-2.33038894229026,
20.0596438026594));
#12980=CARTESIAN_POINT('Ctrl Pts',(1.76383231338145,-1.56450675022861,20.1866611225834));
#12981=CARTESIAN_POINT('Ctrl Pts',(2.27102180036648,0.633439644702114,20.3136784425075));
#12982=CARTESIAN_POINT('Ctrl Pts',(0.699441717491183,2.25156991564901,20.4406957624314));
#12983=CARTESIAN_POINT('Ctrl Pts',(-1.51236918924863,1.80873581174778,20.5677130823555));
#12984=CARTESIAN_POINT('Ctrl Pts',(-2.33983977455391,-0.289716465807172,
20.6947304022795));
#12985=CARTESIAN_POINT('Ctrl Pts',(-1.02554856753737,-2.12297808204117,
20.8217477222035));
#12986=CARTESIAN_POINT('Ctrl Pts',(1.22747389894261,-2.0129812788532,20.9487650421275));
#12987=CARTESIAN_POINT('Ctrl Pts',(2.35693366377738,-0.0604111340540538,
21.0757823620516));
#12988=CARTESIAN_POINT('Ctrl Pts',(1.32898482224672,1.94745606972551,21.2027996819756));
#12989=CARTESIAN_POINT('Ctrl Pts',(-0.915444287757947,2.1727281375204,21.3298170018996));
#12990=CARTESIAN_POINT('Ctrl Pts',(-2.32192559293657,0.40920329560084,21.4568343218236));
#12991=CARTESIAN_POINT('Ctrl Pts',(-1.60304277450666,-1.72888393657267,
21.5838516417477));
#12992=CARTESIAN_POINT('Ctrl Pts',(0.583178029368184,-2.28444505330724,
21.7108689616716));
#12993=CARTESIAN_POINT('Ctrl Pts',(2.23558944009154,-0.748949678226114,
21.8378862815957));
#12994=CARTESIAN_POINT('Ctrl Pts',(1.84166415556682,1.47209339446037,21.9649036015196));
#12995=CARTESIAN_POINT('Ctrl Pts',(-0.23802015814085,2.34566244151516,22.0919209214437));
#12996=CARTESIAN_POINT('Ctrl Pts',(-2.09983370816391,1.07213988989037,22.2189382413677));
#12997=CARTESIAN_POINT('Ctrl Pts',(-2.0395740982221,-1.18276097452655,22.3459555612917));
#12998=CARTESIAN_POINT('Ctrl Pts',(-0.112399222395231,-2.35502710849036,
22.4729728812157));
#12999=CARTESIAN_POINT('Ctrl Pts',(1.91765919019992,-1.37162941700542,22.5999902011398));
#13000=CARTESIAN_POINT('Ctrl Pts',(2.19239801962464,0.867282364654784,22.7270075210638));
#13001=CARTESIAN_POINT('Ctrl Pts',(0.460333080665931,2.31233250434551,22.8540248409878));
#13002=CARTESIAN_POINT('Ctrl Pts',(-1.69309162754269,1.64079691360341,22.9810421609118));
#13003=CARTESIAN_POINT('Ctrl Pts',(-2.29676024272747,-0.532629796744884,
23.1080594808358));
#13004=CARTESIAN_POINT('Ctrl Pts',(-0.798085058971124,-2.21852563316919,
23.2350768007599));
#13005=CARTESIAN_POINT('Ctrl Pts',(1.43108576045911,-1.87368610656973,23.3620941206838));
#13006=CARTESIAN_POINT('Ctrl Pts',(2.35037186943588,0.186189415184726,23.4891114406079));
#13007=CARTESIAN_POINT('Ctrl Pts',(1.11815436836127,2.07570231768813,23.6161287605319));
#13008=CARTESIAN_POINT('Ctrl Pts',(-1.13736772283233,2.06510660675428,23.7431460804559));
#13009=CARTESIAN_POINT('Ctrl Pts',(-2.3521729797966,0.164460801615943,23.8701634003799));
#13010=CARTESIAN_POINT('Ctrl Pts',(-1.41322686604255,-1.88717311423397,
23.9971807203039));
#13011=CARTESIAN_POINT('Ctrl Pts',(0.817973374160278,-2.21053272043233,
24.1241980402279));
#13012=CARTESIAN_POINT('Ctrl Pts',(2.30301402245599,-0.512148340557086,
24.2512153601519));
#13013=CARTESIAN_POINT('Ctrl Pts',(1.674912756705,1.65836796725257,24.378232680076));
#13014=CARTESIAN_POINT('Ctrl Pts',(0.24166366648125,2.0882081993032,24.4629108933587));
#13015=CARTESIAN_POINT('Ctrl Pts',(-0.4076525627588,1.95265126189399,24.50525));
#13016=CARTESIAN_POINT('Ctrl Pts',(-0.941790067967272,1.92904360906019,
-0.175418256788786));
#13017=CARTESIAN_POINT('Ctrl Pts',(-1.58325603104951,1.61586962474357,-0.133079150147447));
#13018=CARTESIAN_POINT('Ctrl Pts',(-2.51814382549676,0.304775439156526,
-0.0484009368647695));
#13019=CARTESIAN_POINT('Ctrl Pts',(-1.62002370869527,-1.95494152338182,
0.0786163830592463));
#13020=CARTESIAN_POINT('Ctrl Pts',(0.76310054745868,-2.41901532289923,0.205633702983263));
#13021=CARTESIAN_POINT('Ctrl Pts',(2.44663379040036,-0.671958019230885,
0.332651022907279));
#13022=CARTESIAN_POINT('Ctrl Pts',(1.8912215416169,1.69178520581912,0.459668342831296));
#13023=CARTESIAN_POINT('Ctrl Pts',(-0.395610621803758,2.50611603743205,
0.586685662755312));
#13024=CARTESIAN_POINT('Ctrl Pts',(-2.32016554568208,1.02692796203862,0.713702982679328));
#13025=CARTESIAN_POINT('Ctrl Pts',(-2.12104973390752,-1.39248661246172,
0.840720302603345));
#13026=CARTESIAN_POINT('Ctrl Pts',(0.0196026223576674,-2.53717271604696,
0.967737622527361));
#13027=CARTESIAN_POINT('Ctrl Pts',(2.1422891101168,-1.35953332690082,1.09475494245138));
#13028=CARTESIAN_POINT('Ctrl Pts',(2.30405283197173,1.06258242927079,1.22177226237539));
#13029=CARTESIAN_POINT('Ctrl Pts',(0.35680592182702,2.51205047367911,1.34878958229941));
#13030=CARTESIAN_POINT('Ctrl Pts',(-1.91703839615649,1.66213371759669,1.47580690222343));
#13031=CARTESIAN_POINT('Ctrl Pts',(-2.43613198247962,-0.709214517731593,
1.60282422214744));
#13032=CARTESIAN_POINT('Ctrl Pts',(-0.725322232454721,-2.43138388276806,
1.72984154207146));
#13033=CARTESIAN_POINT('Ctrl Pts',(1.64940747879268,-1.92799831142548,1.85685886199548));
#13034=CARTESIAN_POINT('Ctrl Pts',(2.51435973748759,0.340172530179638,1.98387618191949));
#13035=CARTESIAN_POINT('Ctrl Pts',(1.07780401121893,2.29696760921754,2.11089350184351));
#13036=CARTESIAN_POINT('Ctrl Pts',(-1.34531469045259,2.15124393353062,2.23791082176752));
#13037=CARTESIAN_POINT('Ctrl Pts',(-2.53700568943262,0.0363887165287244,
2.36492814169154));
#13038=CARTESIAN_POINT('Ctrl Pts',(-1.40645994546512,-2.11177469457974,
2.49194546161556));
#13039=CARTESIAN_POINT('Ctrl Pts',(1.011482560961,-2.32693468452654,2.61896278153957));
#13040=CARTESIAN_POINT('Ctrl Pts',(2.50356906901209,-0.412145483309817,
2.74598010146359));
#13041=CARTESIAN_POINT('Ctrl Pts',(1.70402491014309,1.87989922083475,2.8729974213876));
#13042=CARTESIAN_POINT('Ctrl Pts',(-0.655290769044694,2.45118664963297,
3.00001474131162));
#13043=CARTESIAN_POINT('Ctrl Pts',(-2.41478899682385,0.778791423618739,
3.12703206123564));
#13044=CARTESIAN_POINT('Ctrl Pts',(-1.96392099899146,-1.60646702100726,
3.25404938115965));
#13045=CARTESIAN_POINT('Ctrl Pts',(0.284613234013536,-2.521253118607,3.38106670108367));
#13046=CARTESIAN_POINT('Ctrl Pts',(2.27262802607538,-1.12822153662387,3.50808402100769));
#13047=CARTESIAN_POINT('Ctrl Pts',(2.18040299674552,1.29752254404997,3.6351013409317));
#13048=CARTESIAN_POINT('Ctrl Pts',(0.0923559110667471,2.53558521181829,
3.76211866085572));
#13049=CARTESIAN_POINT('Ctrl Pts',(-2.08022874159101,1.45271138333953,3.88913598077973));
#13050=CARTESIAN_POINT('Ctrl Pts',(-2.34868539084933,-0.959895262741452,
4.01615330070375));
#13051=CARTESIAN_POINT('Ctrl Pts',(-0.4672834527091,-2.49386610616313,4.14317062062777));
#13052=CARTESIAN_POINT('Ctrl Pts',(1.84184428790656,-1.74508784871679,4.27018794055178));
#13053=CARTESIAN_POINT('Ctrl Pts',(2.46504816045325,0.601048706245761,4.3972052604758));
#13054=CARTESIAN_POINT('Ctrl Pts',(0.831881308867185,2.3970180367686,4.52422258039981));
#13055=CARTESIAN_POINT('Ctrl Pts',(-1.56274434964838,1.99888771027209,4.65123990032383));
#13056=CARTESIAN_POINT('Ctrl Pts',(-2.52691901072642,-0.228915473186961,
4.77825722024785));
#13057=CARTESIAN_POINT('Ctrl Pts',(-1.17808974371463,-2.24718190994627,
4.90527454017187));
#13058=CARTESIAN_POINT('Ctrl Pts',(1.24909866076361,-2.20850051308883,5.03229186009588));
#13059=CARTESIAN_POINT('Ctrl Pts',(2.5329302355793,-0.148278124898084,5.1593091800199));
#13060=CARTESIAN_POINT('Ctrl Pts',(1.49825553472755,2.0476699766548,5.28632649994391));
#13061=CARTESIAN_POINT('Ctrl Pts',(-0.907840617463509,2.36929259356429,
5.41334381986794));
#13062=CARTESIAN_POINT('Ctrl Pts',(-2.48294895193696,0.522193912938763,
5.54036113979194));
#13063=CARTESIAN_POINT('Ctrl Pts',(-1.78530115346812,-1.80289261245937,
5.66737845971597));
#13064=CARTESIAN_POINT('Ctrl Pts',(0.546514009790199,-2.47770951036197,
5.79439577963998));
#13065=CARTESIAN_POINT('Ctrl Pts',(2.37808003722935,-0.884566174554725,
5.921413099564));
#13066=CARTESIAN_POINT('Ctrl Pts',(2.03288122017812,1.51826082254739,6.04843041948801));
#13067=CARTESIAN_POINT('Ctrl Pts',(-0.173106259925872,2.53135461826462,
6.17544773941203));
#13068=CARTESIAN_POINT('Ctrl Pts',(-2.22064170516612,1.22738437252235,6.30246505933605));
#13069=CARTESIAN_POINT('Ctrl Pts',(-2.23552277362324,-1.20006662700327,
6.42948237926006));
#13070=CARTESIAN_POINT('Ctrl Pts',(-0.204128146351376,-2.52904204799016,
6.55649969918408));
#13071=CARTESIAN_POINT('Ctrl Pts',(2.01411425971366,-1.54307022829594,6.68351701910809));
#13072=CARTESIAN_POINT('Ctrl Pts',(2.38874625540769,0.85534397052349,6.81053433903211));
#13073=CARTESIAN_POINT('Ctrl Pts',(0.576850131872557,2.47082292080873,6.93755165895612));
#13074=CARTESIAN_POINT('Ctrl Pts',(-1.76306316011027,1.82464524609501,7.06456897888015));
#13075=CARTESIAN_POINT('Ctrl Pts',(-2.48916453430101,-0.491713231277311,
7.19158629880415));
#13076=CARTESIAN_POINT('Ctrl Pts',(-0.936820370245068,-2.3579842184648,
7.31860361872818));
#13077=CARTESIAN_POINT('Ctrl Pts',(1.47303809763044,-2.06588497829972,7.44562093865219));
#13078=CARTESIAN_POINT('Ctrl Pts',(2.53455778156296,0.11721276617261,7.57263825857621));
#13079=CARTESIAN_POINT('Ctrl Pts',(1.27608142294691,2.19302033338612,7.69965557850022));
#13080=CARTESIAN_POINT('Ctrl Pts',(-1.15045031508959,2.26145662199066,7.82667289842425));
#13081=CARTESIAN_POINT('Ctrl Pts',(-2.52392254208557,0.259878783642378,
7.95369021834826));
#13082=CARTESIAN_POINT('Ctrl Pts',(-1.58713364505749,-1.97957792808509,
8.08070753827228));
#13083=CARTESIAN_POINT('Ctrl Pts',(0.802430881042418,-2.40703690494862,
8.20772485819628));
#13084=CARTESIAN_POINT('Ctrl Pts',(2.45749391659467,-0.63122549895843,8.33474217812031));
#13085=CARTESIAN_POINT('Ctrl Pts',(1.86310097108385,1.72237532268131,8.46175949804432));
#13086=CARTESIAN_POINT('Ctrl Pts',(-0.436673051640951,2.49940765514666,
8.58877681796835));
#13087=CARTESIAN_POINT('Ctrl Pts',(-2.33674036455467,0.988618454863179,
8.71579413789234));
#13088=CARTESIAN_POINT('Ctrl Pts',(-2.09788291605014,-1.42709819255022,
8.84281145781638));
#13089=CARTESIAN_POINT('Ctrl Pts',(0.061262204872421,-2.53652694109274,
8.96982877774038));
#13090=CARTESIAN_POINT('Ctrl Pts',(2.16433124266297,-1.32415718578578,9.09684609766441));
#13091=CARTESIAN_POINT('Ctrl Pts',(2.28628943174133,1.10027388178719,9.22386341758841));
#13092=CARTESIAN_POINT('Ctrl Pts',(0.315502893378693,2.51757421040668,9.35088073751245));
#13093=CARTESIAN_POINT('Ctrl Pts',(-1.94407779652221,1.63042433179356,9.47789805743645));
#13094=CARTESIAN_POINT('Ctrl Pts',(-2.42415563699242,-0.749127110891748,
9.60491537736048));
#13095=CARTESIAN_POINT('Ctrl Pts',(-0.685293540383725,-2.44296842880613,
9.73193269728448));
#13096=CARTESIAN_POINT('Ctrl Pts',(1.68084890991805,-1.90064960544086,9.85895001720851));
#13097=CARTESIAN_POINT('Ctrl Pts',(2.50843388581605,0.381420268372014,9.98596733713252));
#13098=CARTESIAN_POINT('Ctrl Pts',(1.03993520940162,2.31435881852446,10.1129846570565));
#13099=CARTESIAN_POINT('Ctrl Pts',(-1.38046347413391,2.12885945454773,10.2400019769806));
#13100=CARTESIAN_POINT('Ctrl Pts',(-2.53726113812648,-0.00528181675498858,
10.3670192969046));
#13101=CARTESIAN_POINT('Ctrl Pts',(-1.37158825432365,-2.13458840089526,
10.4940366168286));
#13102=CARTESIAN_POINT('Ctrl Pts',(1.04956175656788,-2.31000911248967,10.6210539367526));
#13103=CARTESIAN_POINT('Ctrl Pts',(2.5100001437748,-0.370973393770508,10.7480712566766));
#13104=CARTESIAN_POINT('Ctrl Pts',(1.67292121150563,1.9076311490248,10.8750885766006));
#13105=CARTESIAN_POINT('Ctrl Pts',(-0.695458612154235,2.44009411691755,
11.0021058965247));
#13106=CARTESIAN_POINT('Ctrl Pts',(-2.42725352948809,0.739027931963853,
11.1291232164487));
#13107=CARTESIAN_POINT('Ctrl Pts',(-1.93727286780878,-1.63850413984437,
11.2561405363727));
#13108=CARTESIAN_POINT('Ctrl Pts',(0.325981782472021,-2.51623883169534,
11.3831578562967));
#13109=CARTESIAN_POINT('Ctrl Pts',(2.29085047730947,-1.0907456491988,11.5101751762207));
#13110=CARTESIAN_POINT('Ctrl Pts',(2.15879951220094,1.3331566474935,11.6371924961447));
#13111=CARTESIAN_POINT('Ctrl Pts',(0.0507011429281111,2.53676001520462,
11.7642098160688));
#13112=CARTESIAN_POINT('Ctrl Pts',(-2.10380628902285,1.41835153572837,11.8912271359927));
#13113=CARTESIAN_POINT('Ctrl Pts',(-2.33260411580082,-0.998338629716504,
12.0182444559168));
#13114=CARTESIAN_POINT('Ctrl Pts',(-0.426263277816043,-2.50120402978659,
12.1452617758408));
#13115=CARTESIAN_POINT('Ctrl Pts',(1.8702557304242,-1.71460359367715,12.2722790957648));
#13116=CARTESIAN_POINT('Ctrl Pts',(2.45484458473353,0.641451514488535,12.3992964156888));
#13117=CARTESIAN_POINT('Ctrl Pts',(0.792402511958804,2.41035686977603,12.5263137356129));
#13118=CARTESIAN_POINT('Ctrl Pts',(-1.59536162891899,1.97295292736753,12.6533310555369));
#13119=CARTESIAN_POINT('Ctrl Pts',(-2.52281869277939,-0.270384585355824,
12.7803483754609));
#13120=CARTESIAN_POINT('Ctrl Pts',(-1.14102503610327,-2.26622678644938,
12.9073656953849));
#13121=CARTESIAN_POINT('Ctrl Pts',(1.28520074497129,-2.1876885120511,13.0343830153089));
#13122=CARTESIAN_POINT('Ctrl Pts',(2.53502381630957,-0.106659417673314,
13.1614003352329));
#13123=CARTESIAN_POINT('Ctrl Pts',(1.46442426229433,2.07199989397656,13.2884176551569));
#13124=CARTESIAN_POINT('Ctrl Pts',(-0.946629440310036,2.35406344081323,
13.415434975081));
#13125=CARTESIAN_POINT('Ctrl Pts',(-2.49119015101862,0.481345626450458,
13.542452295005));
#13126=CARTESIAN_POINT('Ctrl Pts',(-1.75545118434715,-1.83196973774387,
13.669469614929));
#13127=CARTESIAN_POINT('Ctrl Pts',(0.587132112407456,-2.46839985885899,
13.796486934853));
#13128=CARTESIAN_POINT('Ctrl Pts',(2.39228667617082,-0.84539129381056,13.923504254777));
#13129=CARTESIAN_POINT('Ctrl Pts',(2.00767241251555,1.55144238199786,14.050521574701));
#13130=CARTESIAN_POINT('Ctrl Pts',(-0.214655745710225,2.52817026552183,
14.1775388946251));
#13131=CARTESIAN_POINT('Ctrl Pts',(-2.24049973451574,1.19074889051809,14.3045562145491));
#13132=CARTESIAN_POINT('Ctrl Pts',(-2.21551238886959,-1.23661911492606,
14.4315735344731));
#13133=CARTESIAN_POINT('Ctrl Pts',(-0.162565762995435,-2.53205338674698,
14.5585908543971));
#13134=CARTESIAN_POINT('Ctrl Pts',(2.03918470138136,-1.5097840025273,14.6856081743211));
#13135=CARTESIAN_POINT('Ctrl Pts',(2.37437663959469,0.8944593640754,14.8126254942451));
#13136=CARTESIAN_POINT('Ctrl Pts',(0.536193621651962,2.47996338294236,14.9396428141691));
#13137=CARTESIAN_POINT('Ctrl Pts',(-1.79279181133975,1.79544409599081,15.0666601340932));
#13138=CARTESIAN_POINT('Ctrl Pts',(-2.48075333961828,-0.532526852475886,
15.1936774540172));
#13139=CARTESIAN_POINT('Ctrl Pts',(-0.897968478795187,-2.37305174653345,
15.3206947739412));
#13140=CARTESIAN_POINT('Ctrl Pts',(1.50676778210746,-2.04141441932747,15.4477120938652));
#13141=CARTESIAN_POINT('Ctrl Pts',(2.5322909443948,0.158822396315005,15.5747294137892));
#13142=CARTESIAN_POINT('Ctrl Pts',(1.23989300331923,2.21368184727507,15.7017467337132));
#13143=CARTESIAN_POINT('Ctrl Pts',(-1.18743541036541,2.24225759600574,15.8287640536373));
#13144=CARTESIAN_POINT('Ctrl Pts',(-2.52785017273414,0.218392959692267,
15.9557813735613));
#13145=CARTESIAN_POINT('Ctrl Pts',(-1.55440867206576,-2.00537668801696,
16.0827986934853));
#13146=CARTESIAN_POINT('Ctrl Pts',(0.841853801132134,-2.39353382222907,
16.2098160134093));
#13147=CARTESIAN_POINT('Ctrl Pts',(2.46752919155041,-0.590780559498783,
16.3368333333333));
#13148=CARTESIAN_POINT('Ctrl Pts',(1.83456285720209,1.75274102582488,16.4638506532573));
#13149=CARTESIAN_POINT('Ctrl Pts',(-0.477662320434784,2.49189901245456,
16.5908679731814));
#13150=CARTESIAN_POINT('Ctrl Pts',(-2.35266144580155,0.950108468583519,
16.7178852931054));
#13151=CARTESIAN_POINT('Ctrl Pts',(-2.07416251978425,-1.46135958003407,
16.8449026130294));
#13152=CARTESIAN_POINT('Ctrl Pts',(0.10291172083272,-2.53517872315748,16.9719199329534));
#13153=CARTESIAN_POINT('Ctrl Pts',(2.18578618159046,-1.28843344764227,17.0989372528774));
#13154=CARTESIAN_POINT('Ctrl Pts',(2.26791111198236,1.13767357742987,17.2259545728015));
#13155=CARTESIAN_POINT('Ctrl Pts',(0.274113827096781,2.52241622069584,17.3529718927254));
#13156=CARTESIAN_POINT('Ctrl Pts',(-1.97059231403915,1.5982765444331,17.4799892126495));
#13157=CARTESIAN_POINT('Ctrl Pts',(-2.41152566163149,-0.788838363625875,
17.6070065325735));
#13158=CARTESIAN_POINT('Ctrl Pts',(-0.645079863170469,-2.45389363069533,
17.7340238524975));
#13159=CARTESIAN_POINT('Ctrl Pts',(1.71183688078241,-1.87278842217381,17.8610411724215));
#13160=CARTESIAN_POINT('Ctrl Pts',(2.50183145085816,0.422565228257236,17.9880584923455));
#13161=CARTESIAN_POINT('Ctrl Pts',(1.0017858777042,2.33112570143001,18.1150758122696));
#13162=CARTESIAN_POINT('Ctrl Pts',(-1.41523988373396,2.10590076977141,18.2420931321935));
#13163=CARTESIAN_POINT('Ctrl Pts',(-2.5368321958329,-0.0469509405739145,
18.3691104521176));
#13164=CARTESIAN_POINT('Ctrl Pts',(-1.33634659053169,-2.15682631906453,
18.4961277720416));
#13165=CARTESIAN_POINT('Ctrl Pts',(1.08735784373419,-2.29246044683542,18.6231450919656));
#13166=CARTESIAN_POINT('Ctrl Pts',(2.5157541762681,-0.329701236310608,18.7501624118896));
#13167=CARTESIAN_POINT('Ctrl Pts',(1.64136626161557,1.93484851496579,18.8771797318136));
#13168=CARTESIAN_POINT('Ctrl Pts',(-0.735438863258405,2.42834339808939,
19.0041970517377));
#13169=CARTESIAN_POINT('Ctrl Pts',(-2.4390633391421,0.699065095887472,19.1312143716617));
#13170=CARTESIAN_POINT('Ctrl Pts',(-1.91010217997055,-1.6700992912719,19.2582316915857));
#13171=CARTESIAN_POINT('Ctrl Pts',(0.36726240114322,-2.5105458190086,19.3852490115097));
#13172=CARTESIAN_POINT('Ctrl Pts',(2.30845499855749,-1.05297554590326,19.5122663314337));
#13173=CARTESIAN_POINT('Ctrl Pts',(2.13661371684177,1.36843114756956,19.6392836513577));
#13174=CARTESIAN_POINT('Ctrl Pts',(0.00903269875653687,2.53725055739237,
19.7663009712818));
#13175=CARTESIAN_POINT('Ctrl Pts',(-2.12681635942717,1.38360910444733,19.8933182912058));
#13176=CARTESIAN_POINT('Ctrl Pts',(-2.31589364819477,-1.0365127065718,20.0203356111298));
#13177=CARTESIAN_POINT('Ctrl Pts',(-0.385128123413262,-2.50786728300945,
20.1473529310538));
#13178=CARTESIAN_POINT('Ctrl Pts',(1.89816269343304,-1.68365684446206,20.2743702509778));
#13179=CARTESIAN_POINT('Ctrl Pts',(2.44397884352426,0.681681298722785,20.4013875709018));
#13180=CARTESIAN_POINT('Ctrl Pts',(0.752709973788363,2.42304553733211,20.5284048908259));
#13181=CARTESIAN_POINT('Ctrl Pts',(-1.62754857814452,1.94648596359704,20.6554222107499));
#13182=CARTESIAN_POINT('Ctrl Pts',(-2.51803787410739,-0.311780764473142,
20.7824395306739));
#13183=CARTESIAN_POINT('Ctrl Pts',(-1.10365255043497,-2.28466037487492,
20.9094568505979));
#13184=CARTESIAN_POINT('Ctrl Pts',(1.32095616145559,-2.16628640778953,21.0364741705219));
#13185=CARTESIAN_POINT('Ctrl Pts',(2.53643360399821,-0.065011940227747,
21.1634914904459));
#13186=CARTESIAN_POINT('Ctrl Pts',(1.43019797890608,2.09577091348664,21.29050881037));
#13187=CARTESIAN_POINT('Ctrl Pts',(-0.985162921529244,2.33819930745395,
21.417526130294));
#13188=CARTESIAN_POINT('Ctrl Pts',(-2.49875937979054,0.440367501970874,
21.544543450218));
#13189=CARTESIAN_POINT('Ctrl Pts',(-1.72512770486239,-1.86055270945033,
21.671560770142));
#13190=CARTESIAN_POINT('Ctrl Pts',(0.627591846786366,-2.45842438790134,
21.798578090066));
#13191=CARTESIAN_POINT('Ctrl Pts',(2.40584801674221,-0.805988374111369,
21.9255954099901));
#13192=CARTESIAN_POINT('Ctrl Pts',(1.98192207241512,1.58420544935872,22.052612729914));
#13193=CARTESIAN_POINT('Ctrl Pts',(-0.256147356548822,2.52430398518738,
22.1796300498381));
#13194=CARTESIAN_POINT('Ctrl Pts',(-2.25975336601507,1.15379218630468,22.3066473697621));
#13195=CARTESIAN_POINT('Ctrl Pts',(-2.19490448971053,-1.27283797902012,
22.4336646896861));
#13196=CARTESIAN_POINT('Ctrl Pts',(-0.120959350332131,-2.53438184879942,
22.5606820096101));
#13197=CARTESIAN_POINT('Ctrl Pts',(2.06370475579857,-1.47609031131966,22.6876993295342));
#13198=CARTESIAN_POINT('Ctrl Pts',(2.3593672133321,0.933333070706771,22.8147166494581));
#13199=CARTESIAN_POINT('Ctrl Pts',(0.495391241924784,2.48843569837242,22.9417339693822));
#13200=CARTESIAN_POINT('Ctrl Pts',(-1.8220345208464,1.76575713307529,23.0687512893062));
#13201=CARTESIAN_POINT('Ctrl Pts',(-2.47167748058067,-0.573193949289761,
23.1957686092302));
#13202=CARTESIAN_POINT('Ctrl Pts',(-0.858865819404909,-2.38748466016789,
23.3227859291542));
#13203=CARTESIAN_POINT('Ctrl Pts',(1.54007474576711,-2.01638275912753,23.4498032490782));
#13204=CARTESIAN_POINT('Ctrl Pts',(2.5293720748911,0.20036927497846,23.5768205690023));
#13205=CARTESIAN_POINT('Ctrl Pts',(1.20331104687244,2.23378417110109,23.7038378889263));
#13206=CARTESIAN_POINT('Ctrl Pts',(-1.22398765677242,2.22238150937836,23.8308552088503));
#13207=CARTESIAN_POINT('Ctrl Pts',(-2.53131035466268,0.17698584825274,23.9578725287743));
#13208=CARTESIAN_POINT('Ctrl Pts',(-1.52085574922736,-2.03089691367622,
24.0848898486983));
#13209=CARTESIAN_POINT('Ctrl Pts',(0.880268793849252,-2.37888302119466,
24.2119071686224));
#13210=CARTESIAN_POINT('Ctrl Pts',(2.47840753722132,-0.551152661267064,
24.3389244885463));
#13211=CARTESIAN_POINT('Ctrl Pts',(1.80247117904166,1.78466636739888,24.4659418084704));
#13212=CARTESIAN_POINT('Ctrl Pts',(0.260068348103614,2.24724247875885,24.550620021753));
#13213=CARTESIAN_POINT('Ctrl Pts',(-0.438698668031391,2.10136176239249,
24.5929591283944));
#13214=CARTESIAN_POINT('Ctrl Pts',(-1.00843926415924,2.06555938931316,-0.0877091283943953));
#13215=CARTESIAN_POINT('Ctrl Pts',(-1.69530089691146,1.73022251006604,-0.0453700217530565));
#13216=CARTESIAN_POINT('Ctrl Pts',(-2.6963494230853,0.326343980522267,0.0393081915296206));
#13217=CARTESIAN_POINT('Ctrl Pts',(-1.73467057286262,-2.09329006364291,
0.166325511453637));
#13218=CARTESIAN_POINT('Ctrl Pts',(0.817104130456275,-2.59020573181402,
0.293342831377653));
#13219=CARTESIAN_POINT('Ctrl Pts',(2.6197787205207,-0.719511570048316,0.42036015130167));
#13220=CARTESIAN_POINT('Ctrl Pts',(2.02506070583922,1.81151053307878,0.547377471225686));
#13221=CARTESIAN_POINT('Ctrl Pts',(-0.423607444922901,2.68347044489473,
0.674394791149703));
#13222=CARTESIAN_POINT('Ctrl Pts',(-2.48436049093747,1.09960225065647,0.801412111073719));
#13223=CARTESIAN_POINT('Ctrl Pts',(-2.27115352524731,-1.49103098724893,
0.928429430997735));
#13224=CARTESIAN_POINT('Ctrl Pts',(0.0209898731557613,-2.71672496221751,
1.05544675092175));
#13225=CARTESIAN_POINT('Ctrl Pts',(2.29389598308821,-1.45574564269816,1.18246407084577));
#13226=CARTESIAN_POINT('Ctrl Pts',(2.46710750249518,1.13777993581432,1.30948139076978));
#13227=CARTESIAN_POINT('Ctrl Pts',(0.382056589353797,2.68982485308583,1.4364987106938));
#13228=CARTESIAN_POINT('Ctrl Pts',(-2.05270458389693,1.77976064955236,1.56351603061782));
#13229=CARTESIAN_POINT('Ctrl Pts',(-2.60853371400369,-0.759404660038483,
1.69053335054183));
#13230=CARTESIAN_POINT('Ctrl Pts',(-0.776652295721961,-2.60344959776366,
1.81755067046585));
#13231=CARTESIAN_POINT('Ctrl Pts',(1.76613379221813,-2.06444011739318,1.94456799038987));
#13232=CARTESIAN_POINT('Ctrl Pts',(2.69229754033851,0.364246075308452,2.07158531031388));
#13233=CARTESIAN_POINT('Ctrl Pts',(1.1540787283172,2.45952086820838,2.1986026302379));
#13234=CARTESIAN_POINT('Ctrl Pts',(-1.44052077277774,2.30348452711858,2.32561995016191));
#13235=CARTESIAN_POINT('Ctrl Pts',(-2.71654611535792,0.038963896273717,
2.45263727008594));
#13236=CARTESIAN_POINT('Ctrl Pts',(-1.50599319393492,-2.2612221040603,2.57965459000994));
#13237=CARTESIAN_POINT('Ctrl Pts',(1.08306379965016,-2.49160867248817,2.70667190993397));
#13238=CARTESIAN_POINT('Ctrl Pts',(2.68074323100002,-0.441312455983457,
2.83368922985798));
#13239=CARTESIAN_POINT('Ctrl Pts',(1.82461642455265,2.01293711988686,2.960706549782));
#13240=CARTESIAN_POINT('Ctrl Pts',(-0.701664801341637,2.62465377937989,
3.08772386970601));
#13241=CARTESIAN_POINT('Ctrl Pts',(-2.58568031441742,0.833905428481168,
3.21474118963003));
#13242=CARTESIAN_POINT('Ctrl Pts',(-2.1029050044713,-1.72015449691165,3.34175850955404));
#13243=CARTESIAN_POINT('Ctrl Pts',(0.304754923672212,-2.69967875662022,
3.46877582947807));
#13244=CARTESIAN_POINT('Ctrl Pts',(2.43345880602631,-1.20806423310154,3.59579314940208));
#13245=CARTESIAN_POINT('Ctrl Pts',(2.33470713739251,1.38934644148024,3.72281046932609));
#13246=CARTESIAN_POINT('Ctrl Pts',(0.0988918126922846,2.71502511248385,
3.84982778925011));
#13247=CARTESIAN_POINT('Ctrl Pts',(-2.22744368708483,1.55551778286699,3.97684510917413));
#13248=CARTESIAN_POINT('Ctrl Pts',(-2.51489864657596,-1.02782573882757,
4.10386242909814));
#13249=CARTESIAN_POINT('Ctrl Pts',(-0.500352464133315,-2.67035360272895,
4.23087974902216));
#13250=CARTESIAN_POINT('Ctrl Pts',(1.97218909135587,-1.86858533117836,4.35789706894617));
#13251=CARTESIAN_POINT('Ctrl Pts',(2.63949625037973,0.643584101878016,4.48491438887019));
#13252=CARTESIAN_POINT('Ctrl Pts',(0.890752412363458,2.56665172780235,4.61193170879421));
#13253=CARTESIAN_POINT('Ctrl Pts',(-1.67333763184596,2.14034626212867,4.73894902871823));
#13254=CARTESIAN_POINT('Ctrl Pts',(-2.70574561618272,-0.245115508420684,
4.86596634864224));
#13255=CARTESIAN_POINT('Ctrl Pts',(-1.26146154506521,-2.40621190302983,
4.99298366856626));
#13256=CARTESIAN_POINT('Ctrl Pts',(1.33749566614299,-2.36479307657332,5.12000098849026));
#13257=CARTESIAN_POINT('Ctrl Pts',(2.71218224720435,-0.158771565181015,
5.2470183084143));
#13258=CARTESIAN_POINT('Ctrl Pts',(1.60428503161449,2.19258078284432,5.37403562833829));
#13259=CARTESIAN_POINT('Ctrl Pts',(-0.97208725743388,2.53696419286815,5.50105294826233));
#13260=CARTESIAN_POINT('Ctrl Pts',(-2.65866385641605,0.559148862600505,
5.62807026818633));
#13261=CARTESIAN_POINT('Ctrl Pts',(-1.91164447655709,-1.93048085906317,
5.75508758811036));
#13262=CARTESIAN_POINT('Ctrl Pts',(0.585190059473756,-2.65305362672027,
5.88210490803437));
#13263=CARTESIAN_POINT('Ctrl Pts',(2.54637351191372,-0.947165714003964,
6.00912222795839));
#13264=CARTESIAN_POINT('Ctrl Pts',(2.17674544627999,1.62570606631697,6.1361395478824));
#13265=CARTESIAN_POINT('Ctrl Pts',(-0.185356753398145,2.71049512560532,
6.26315686780642));
#13266=CARTESIAN_POINT('Ctrl Pts',(-2.3777934842235,1.31424468739453,6.39017418773043));
#13267=CARTESIAN_POINT('Ctrl Pts',(-2.39372766556092,-1.28499370235373,
6.51719150765445));
#13268=CARTESIAN_POINT('Ctrl Pts',(-0.218574016335755,-2.70801889789258,
6.64420882757846));
#13269=CARTESIAN_POINT('Ctrl Pts',(2.15665037366779,-1.65227119980924,6.7712261475025));
#13270=CARTESIAN_POINT('Ctrl Pts',(2.55779456377756,0.915875494524468,6.8982434674265));
#13271=CARTESIAN_POINT('Ctrl Pts',(0.617673027462724,2.6456796826346,7.02526078735052));
#13272=CARTESIAN_POINT('Ctrl Pts',(-1.88783273079667,1.95377289685707,7.15227810727453));
#13273=CARTESIAN_POINT('Ctrl Pts',(-2.66531930705065,-0.526511104748562,
7.27929542719855));
#13274=CARTESIAN_POINT('Ctrl Pts',(-1.00311786772006,-2.52485553951532,
7.40631274712256));
#13275=CARTESIAN_POINT('Ctrl Pts',(1.57728299095268,-2.21208483526556,7.53333006704659));
#13276=CARTESIAN_POINT('Ctrl Pts',(2.71392497239329,0.125507753468168,7.66034738697059));
#13277=CARTESIAN_POINT('Ctrl Pts',(1.36638796153508,2.34821738570612,7.78736470689462));
#13278=CARTESIAN_POINT('Ctrl Pts',(-1.2318661118446,2.42149681693976,7.91438202681864));
#13279=CARTESIAN_POINT('Ctrl Pts',(-2.70253709155071,0.278270050046848,
8.04139934674264));
#13280=CARTESIAN_POINT('Ctrl Pts',(-1.69945292436414,-2.11966995304237,
8.16841666666667));
#13281=CARTESIAN_POINT('Ctrl Pts',(0.859217818004418,-2.57737961759307,
8.29543398659068));
#13282=CARTESIAN_POINT('Ctrl Pts',(2.63140740300587,-0.675896464975523,
8.42245130651469));
#13283=CARTESIAN_POINT('Ctrl Pts',(1.99495008095517,1.84426547071115,8.54946862643872));
#13284=CARTESIAN_POINT('Ctrl Pts',(-0.467575806809516,2.67628731956173,
8.67648594636272));
#13285=CARTESIAN_POINT('Ctrl Pts',(-2.50210828709286,1.05858163200661,8.80350326628676));
#13286=CARTESIAN_POINT('Ctrl Pts',(-2.24634722334667,-1.52809198156497,
8.93052058621076));
#13287=CARTESIAN_POINT('Ctrl Pts',(0.0655976473989457,-2.71603348665222,
9.05753790613478));
#13288=CARTESIAN_POINT('Ctrl Pts',(2.31749800723498,-1.41786598041648,9.18455522605879));
#13289=CARTESIAN_POINT('Ctrl Pts',(2.44808701070344,1.17813876092146,9.31157254598281));
#13290=CARTESIAN_POINT('Ctrl Pts',(0.337830602021103,2.69573949711365,9.43858986590683));
#13291=CARTESIAN_POINT('Ctrl Pts',(-2.08165752567829,1.74580723384554,9.56560718583084));
#13292=CARTESIAN_POINT('Ctrl Pts',(-2.59570981891155,-0.802141812877639,
9.69262450575486));
#13293=CARTESIAN_POINT('Ctrl Pts',(-0.733790827810694,-2.61585396629502,
9.81964182567887));
#13294=CARTESIAN_POINT('Ctrl Pts',(1.7998002904608,-2.03515598085693,9.9466591456029));
#13295=CARTESIAN_POINT('Ctrl Pts',(2.68595232424161,0.408412859569337,10.0736764655269));
#13296=CARTESIAN_POINT('Ctrl Pts',(1.11353000314147,2.47814282963356,10.2006937854509));
#13297=CARTESIAN_POINT('Ctrl Pts',(-1.47815698785079,2.27951592914556,10.3277111053749));
#13298=CARTESIAN_POINT('Ctrl Pts',(-2.71681964180679,-0.00565560370938429,
10.454728425299));
#13299=CARTESIAN_POINT('Ctrl Pts',(-1.46865368086213,-2.28565030519776,
10.581745745223));
#13300=CARTESIAN_POINT('Ctrl Pts',(1.12383780789645,-2.47348530084635,10.708763065147));
#13301=CARTESIAN_POINT('Ctrl Pts',(2.68762942413589,-0.397226673927448,
10.835780385071));
#13302=CARTESIAN_POINT('Ctrl Pts',(1.79131155966456,2.04263159874036,10.962797704995));
#13303=CARTESIAN_POINT('Ctrl Pts',(-0.744675267820305,2.6127762432817,11.089815024919));
#13304=CARTESIAN_POINT('Ctrl Pts',(-2.59902694502602,0.791327928857071,
11.2168323448431));
#13305=CARTESIAN_POINT('Ctrl Pts',(-2.07437102145842,-1.75445883887142,
11.3438496647671));
#13306=CARTESIAN_POINT('Ctrl Pts',(0.349051067776654,-2.69430961547564,
11.4708669846911));
#13307=CARTESIAN_POINT('Ctrl Pts',(2.45297083523399,-1.16793622833267,11.5978843046151));
#13308=CARTESIAN_POINT('Ctrl Pts',(2.31157480376701,1.42750232173191,11.7249016245391));
#13309=CARTESIAN_POINT('Ctrl Pts',(0.0542891935320357,2.7162830551005,11.8519189444631));
#13310=CARTESIAN_POINT('Ctrl Pts',(-2.25268978533066,1.51872633579173,11.9789362643872));
#13311=CARTESIAN_POINT('Ctrl Pts',(-2.49767932166667,-1.06898969035214,
12.1059535843112));
#13312=CARTESIAN_POINT('Ctrl Pts',(-0.456429347515495,-2.67821082118026,
12.2329709042352));
#13313=CARTESIAN_POINT('Ctrl Pts',(2.00261117283739,-1.83594374706507,12.3599882241592));
#13314=CARTESIAN_POINT('Ctrl Pts',(2.62857058154909,0.686846161651322,12.4870055440832));
#13315=CARTESIAN_POINT('Ctrl Pts',(0.848479754944057,2.58093453179474,12.6140228640072));
#13316=CARTESIAN_POINT('Ctrl Pts',(-1.70826319140036,2.11257611007679,12.7410401839312));
#13317=CARTESIAN_POINT('Ctrl Pts',(-2.70135512433749,-0.289519332991871,
12.8680575038553));
#13318=CARTESIAN_POINT('Ctrl Pts',(-1.22177381874362,-2.42660455941901,
12.9950748237793));
#13319=CARTESIAN_POINT('Ctrl Pts',(1.37615264551801,-2.34250823866091,13.1220921437033));
#13320=CARTESIAN_POINT('Ctrl Pts',(2.7144239877821,-0.11420755891623,13.2491094636273));
#13321=CARTESIAN_POINT('Ctrl Pts',(1.56805956626024,2.21863249516909,13.3761267835513));
#13322=CARTESIAN_POINT('Ctrl Pts',(-1.0136211122699,2.52065729378692,13.5031441034754));
#13323=CARTESIAN_POINT('Ctrl Pts',(-2.66748827389544,0.515409798694957,
13.6301614233994));
#13324=CARTESIAN_POINT('Ctrl Pts',(-1.8796820659102,-1.96161573277134,13.7571787433234));
#13325=CARTESIAN_POINT('Ctrl Pts',(0.628682649710236,-2.64308514390169,
13.8841960632474));
#13326=CARTESIAN_POINT('Ctrl Pts',(2.56158553528029,-0.905218480480427,
14.0112133831714));
#13327=CARTESIAN_POINT('Ctrl Pts',(2.14975264574595,1.66123583938849,14.1382307030954));
#13328=CARTESIAN_POINT('Ctrl Pts',(-0.229846639515761,2.70708542057022,
14.2652480230195));
#13329=CARTESIAN_POINT('Ctrl Pts',(-2.399056839175,1.27501656238973,14.3922653429435));
#13330=CARTESIAN_POINT('Ctrl Pts',(-2.37230117322164,-1.32413295989931,
14.5192826628675));
#13331=CARTESIAN_POINT('Ctrl Pts',(-0.174070319903033,-2.71124334497834,
14.6462999827915));
#13332=CARTESIAN_POINT('Ctrl Pts',(2.18349501623457,-1.61662935332725,14.7733173027155));
#13333=CARTESIAN_POINT('Ctrl Pts',(2.54240802988898,0.957759031028439,14.9003346226395));
#13334=CARTESIAN_POINT('Ctrl Pts',(0.574139311569299,2.65546700278335,15.0273519425636));
#13335=CARTESIAN_POINT('Ctrl Pts',(-1.91966523805065,1.92250522126218,15.1543692624876));
#13336=CARTESIAN_POINT('Ctrl Pts',(-2.65631286361378,-0.570213050149194,
15.2813865824116));
#13337=CARTESIAN_POINT('Ctrl Pts',(-0.961516481001816,-2.54098937595623,
15.4084039023356));
#13338=CARTESIAN_POINT('Ctrl Pts',(1.61339967910989,-2.18588252827287,15.5354212222596));
#13339=CARTESIAN_POINT('Ctrl Pts',(2.71149771425628,0.17006204027786,15.6624385421836));
#13340=CARTESIAN_POINT('Ctrl Pts',(1.32763853690037,2.37034108669987,15.7894558621077));
#13341=CARTESIAN_POINT('Ctrl Pts',(-1.27146859177446,2.40093910212058,15.9164731820316));
#13342=CARTESIAN_POINT('Ctrl Pts',(-2.70674267525333,0.233848331024494,
16.0434905019557));
#13343=CARTESIAN_POINT('Ctrl Pts',(-1.66441204975114,-2.14729445596166,
16.1705078218797));
#13344=CARTESIAN_POINT('Ctrl Pts',(0.901430644279058,-2.56292094016088,
16.2975251418037));
#13345=CARTESIAN_POINT('Ctrl Pts',(2.64215286065742,-0.632589292416696,
16.4245424617277));
#13346=CARTESIAN_POINT('Ctrl Pts',(1.96439236375018,1.87678011317268,16.5515597816518));
#13347=CARTESIAN_POINT('Ctrl Pts',(-0.511465830145711,2.66824730048656,
16.6785771015757));
#13348=CARTESIAN_POINT('Ctrl Pts',(-2.51915608150405,1.01734634662028,16.8055944214998));
#13349=CARTESIAN_POINT('Ctrl Pts',(-2.22094816705002,-1.56477800062425,
16.9326117414238));
#13350=CARTESIAN_POINT('Ctrl Pts',(0.110194642691373,-2.71458985717596,
17.0596290613478));
#13351=CARTESIAN_POINT('Ctrl Pts',(2.34047128287306,-1.3796141221396,17.1866463812718));
#13352=CARTESIAN_POINT('Ctrl Pts',(2.42840808236836,1.2181851819196,17.3136637011959));
#13353=CARTESIAN_POINT('Ctrl Pts',(0.293512488074909,2.70092416985456,17.4406810211198));
#13354=CARTESIAN_POINT('Ctrl Pts',(-2.11004843936889,1.71138439150223,17.5676983410439));
#13355=CARTESIAN_POINT('Ctrl Pts',(-2.58218603745268,-0.844663376703935,
17.6947156609679));
#13356=CARTESIAN_POINT('Ctrl Pts',(-0.690731283611418,-2.62755232979307,
17.8217329808919));
#13357=CARTESIAN_POINT('Ctrl Pts',(1.83298123767942,-2.00532309972126,17.9487503008159));
#13358=CARTESIAN_POINT('Ctrl Pts',(2.67888264398372,0.45246959204271,18.0757676207399));
#13359=CARTESIAN_POINT('Ctrl Pts',(1.07268089536934,2.49609628193107,18.2027849406639));
#13360=CARTESIAN_POINT('Ctrl Pts',(-1.51539447643767,2.25493248961973,18.329802260588));
#13361=CARTESIAN_POINT('Ctrl Pts',(-2.71636034385321,-0.050273594481799,
18.456819580512));
#13362=CARTESIAN_POINT('Ctrl Pts',(-1.43091801267993,-2.30946197044866,
18.583836900436));
#13363=CARTESIAN_POINT('Ctrl Pts',(1.16430867250469,-2.45469474010331,18.71085422036));
#13364=CARTESIAN_POINT('Ctrl Pts',(2.69379066164609,-0.353033742280847,
18.837871540284));
#13365=CARTESIAN_POINT('Ctrl Pts',(1.75752350908935,2.07177510047756,18.9648888602081));
#13366=CARTESIAN_POINT('Ctrl Pts',(-0.78748486666372,2.60019394213895,19.091906180132));
#13367=CARTESIAN_POINT('Ctrl Pts',(-2.61167251877161,0.748536977479163,
19.2189235000561));
#13368=CARTESIAN_POINT('Ctrl Pts',(-2.04527750116953,-1.78828993599198,
19.3459408199801));
#13369=CARTESIAN_POINT('Ctrl Pts',(0.393253059422915,-2.68821371606033,
19.4729581399041));
#13370=CARTESIAN_POINT('Ctrl Pts',(2.47182120439486,-1.12749318643823,19.5999754598281));
#13371=CARTESIAN_POINT('Ctrl Pts',(2.28781894998626,1.46527314997717,19.7269927797521));
#13372=CARTESIAN_POINT('Ctrl Pts',(0.00967193050468428,2.71680831228858,
19.8540100996762));
#13373=CARTESIAN_POINT('Ctrl Pts',(-2.27732824697515,1.48152523012306,19.9810274196002));
#13374=CARTESIAN_POINT('Ctrl Pts',(-2.47978627710233,-1.10986529446316,
20.1080447395242));
#13375=CARTESIAN_POINT('Ctrl Pts',(-0.412383114445153,-2.68534562372864,
20.2350620594482));
#13376=CARTESIAN_POINT('Ctrl Pts',(2.03249307348463,-1.80280693869551,20.3620793793722));
#13377=CARTESIAN_POINT('Ctrl Pts',(2.61693588668204,0.729922952743455,20.4890966992963));
#13378=CARTESIAN_POINT('Ctrl Pts',(0.805978230085543,2.59452115901522,20.6161140192202));
#13379=CARTESIAN_POINT('Ctrl Pts',(-1.74272796704041,2.08423611544629,20.7431313391443));
#13380=CARTESIAN_POINT('Ctrl Pts',(-2.69623597366087,-0.333845063139111,
20.8701486590683));
#13381=CARTESIAN_POINT('Ctrl Pts',(-1.18175653333257,-2.44634266770867,
20.9971659789923));
#13382=CARTESIAN_POINT('Ctrl Pts',(1.41443842396857,-2.31959153672586,21.1241832989163));
#13383=CARTESIAN_POINT('Ctrl Pts',(2.71593354421905,-0.0696127464014399,
21.2512006188403));
#13384=CARTESIAN_POINT('Ctrl Pts',(1.53141113556543,2.24408575724777,21.3782179387644));
#13385=CARTESIAN_POINT('Ctrl Pts',(-1.05488155530054,2.50367047738749,21.5052352586884));
#13386=CARTESIAN_POINT('Ctrl Pts',(-2.67559316664451,0.471531708340905,
21.6322525786124));
#13387=CARTESIAN_POINT('Ctrl Pts',(-1.84721263521812,-1.99222148232799,
21.7592698985364));
#13388=CARTESIAN_POINT('Ctrl Pts',(0.67200566420455,-2.63240372249544,21.8862872184604));
#13389=CARTESIAN_POINT('Ctrl Pts',(2.57610659339288,-0.863027069996625,
22.0133045383844));
#13390=CARTESIAN_POINT('Ctrl Pts',(2.12217998926342,1.69631750425708,22.1403218583085));
#13391=CARTESIAN_POINT('Ctrl Pts',(-0.274274554956796,2.70294552885961,
22.2673391782324));
#13392=CARTESIAN_POINT('Ctrl Pts',(-2.41967302386623,1.23544448271899,22.3943564981565));
#13393=CARTESIAN_POINT('Ctrl Pts',(-2.35023488119896,-1.36291498351369,
22.5213738180805));
#13394=CARTESIAN_POINT('Ctrl Pts',(-0.129519478269032,-2.71373658910848,
22.6483911380045));
#13395=CARTESIAN_POINT('Ctrl Pts',(2.20975032139722,-1.58055120563391,22.7754084579285));
#13396=CARTESIAN_POINT('Ctrl Pts',(2.52633640703956,0.999383776758762,22.9024257778525));
#13397=CARTESIAN_POINT('Ctrl Pts',(0.530449403183637,2.66453889239932,23.0294430977766));
#13398=CARTESIAN_POINT('Ctrl Pts',(-1.95097741415011,1.89071735254717,23.1564604177006));
#13399=CARTESIAN_POINT('Ctrl Pts',(-2.64659471843386,-0.613758101834641,
23.2834777376246));
#13400=CARTESIAN_POINT('Ctrl Pts',(-0.9196465798387,-2.55644368716658,23.4104950575486));
#13401=CARTESIAN_POINT('Ctrl Pts',(1.64906373107512,-2.15907941168533,23.5375123774727));
#13402=CARTESIAN_POINT('Ctrl Pts',(2.70837228034631,0.214549134772193,23.6645296973966));
#13403=CARTESIAN_POINT('Ctrl Pts',(1.28846772538361,2.39186602451404,23.7915470173207));
#13404=CARTESIAN_POINT('Ctrl Pts',(-1.31060759071252,2.37965641200244,23.9185643372446));
#13405=CARTESIAN_POINT('Ctrl Pts',(-2.71044772952875,0.189510894889534,
24.0455816571687));
#13406=CARTESIAN_POINT('Ctrl Pts',(-1.62848463241217,-2.17462071311847,
24.1725989770927));
#13407=CARTESIAN_POINT('Ctrl Pts',(0.942564213538227,-2.54723332195699,
24.2996162970167));
#13408=CARTESIAN_POINT('Ctrl Pts',(2.65380105198664,-0.590156981977038,
24.4266336169407));
#13409=CARTESIAN_POINT('Ctrl Pts',(1.93002960137832,1.91096476754518,24.5536509368648));
#13410=CARTESIAN_POINT('Ctrl Pts',(0.278473029725979,2.4062767582145,24.6383291501474));
#13411=CARTESIAN_POINT('Ctrl Pts',(-0.469744773303982,2.25007226289099,
24.6806682567888));
#13412=CARTESIAN_POINT('Ctrl Pts',(-1.0750884603512,2.20207516956613,-4.71844785465692E-15));
#13413=CARTESIAN_POINT('Ctrl Pts',(-1.8073457627734,1.84457539538852,0.0423391066413341));
#13414=CARTESIAN_POINT('Ctrl Pts',(-2.87455502067384,0.347912521888007,
0.127017319924011));
#13415=CARTESIAN_POINT('Ctrl Pts',(-1.84931743702996,-2.231638603904,0.254034639848028));
#13416=CARTESIAN_POINT('Ctrl Pts',(0.871107713453866,-2.76139614072881,
0.381051959772044));
#13417=CARTESIAN_POINT('Ctrl Pts',(2.79292365064105,-0.76706512086575,0.508069279696061));
#13418=CARTESIAN_POINT('Ctrl Pts',(2.15889987006154,1.93123586033844,0.635086599620076));
#13419=CARTESIAN_POINT('Ctrl Pts',(-0.451604268042042,2.8608248523574,0.762103919544093));
#13420=CARTESIAN_POINT('Ctrl Pts',(-2.64855543619286,1.17227653927431,0.88912123946811));
#13421=CARTESIAN_POINT('Ctrl Pts',(-2.4212573165871,-1.58957536203614,1.01613855939212));
#13422=CARTESIAN_POINT('Ctrl Pts',(0.0223771239538552,-2.89627720838807,
1.14315587931614));
#13423=CARTESIAN_POINT('Ctrl Pts',(2.44550285605961,-1.5519579584955,1.27017319924016));
#13424=CARTESIAN_POINT('Ctrl Pts',(2.63016217301863,1.21297744235786,1.39719051916418));
#13425=CARTESIAN_POINT('Ctrl Pts',(0.407307256880577,2.86759923249254,1.52420783908819));
#13426=CARTESIAN_POINT('Ctrl Pts',(-2.18837077163737,1.89738758150803,1.65122515901221));
#13427=CARTESIAN_POINT('Ctrl Pts',(-2.78093544552777,-0.809594802345376,
1.77824247893622));
#13428=CARTESIAN_POINT('Ctrl Pts',(-0.8279823589892,-2.77551531275925,1.90525979886024));
#13429=CARTESIAN_POINT('Ctrl Pts',(1.88286010564359,-2.20088192336089,2.03227711878425));
#13430=CARTESIAN_POINT('Ctrl Pts',(2.87023534318944,0.388319620437272,2.15929443870827));
#13431=CARTESIAN_POINT('Ctrl Pts',(1.23035344541546,2.62207412719922,2.28631175863229));
#13432=CARTESIAN_POINT('Ctrl Pts',(-1.53572685510289,2.45572512070654,2.41332907855631));
#13433=CARTESIAN_POINT('Ctrl Pts',(-2.89608654128322,0.0415390760187077,
2.54034639848032));
#13434=CARTESIAN_POINT('Ctrl Pts',(-1.60552644240473,-2.41066951354087,
2.66736371840434));
#13435=CARTESIAN_POINT('Ctrl Pts',(1.15464503833931,-2.65628266044979,2.79438103832835));
#13436=CARTESIAN_POINT('Ctrl Pts',(2.85791739298796,-0.470479428657096,
2.92139835825237));
#13437=CARTESIAN_POINT('Ctrl Pts',(1.94520793896221,2.14597501893897,3.04841567817639));
#13438=CARTESIAN_POINT('Ctrl Pts',(-0.748038833638585,2.79812090912681,
3.1754329981004));
#13439=CARTESIAN_POINT('Ctrl Pts',(-2.75657163201098,0.889019433343594,
3.30245031802442));
#13440=CARTESIAN_POINT('Ctrl Pts',(-2.24188900995115,-1.83384197281603,
3.42946763794843));
#13441=CARTESIAN_POINT('Ctrl Pts',(0.324896613330893,-2.87810439463344,
3.55648495787245));
#13442=CARTESIAN_POINT('Ctrl Pts',(2.59428958597723,-1.2879069295792,3.68350227779647));
#13443=CARTESIAN_POINT('Ctrl Pts',(2.48901127803951,1.48117033891052,3.81051959772048));
#13444=CARTESIAN_POINT('Ctrl Pts',(0.105427714317817,2.8944650131494,3.9375369176445));
#13445=CARTESIAN_POINT('Ctrl Pts',(-2.37465863257865,1.65832418239444,4.06455423756852));
#13446=CARTESIAN_POINT('Ctrl Pts',(-2.68111190230259,-1.09575621491369,
4.19157155749253));
#13447=CARTESIAN_POINT('Ctrl Pts',(-0.533421475557533,-2.84684109929477,
4.31858887741655));
#13448=CARTESIAN_POINT('Ctrl Pts',(2.10253389480519,-1.99208281363993,4.44560619734056));
#13449=CARTESIAN_POINT('Ctrl Pts',(2.8139443403062,0.68611949751027,4.57262351726459));
#13450=CARTESIAN_POINT('Ctrl Pts',(0.949623515859734,2.7362854188361,4.69964083718859));
#13451=CARTESIAN_POINT('Ctrl Pts',(-1.78393091404354,2.28180481398525,4.82665815711262));
#13452=CARTESIAN_POINT('Ctrl Pts',(-2.88457222163901,-0.261315543654406,
4.95367547703663));
#13453=CARTESIAN_POINT('Ctrl Pts',(-1.34483334641579,-2.56524189611339,
5.08069279696065));
#13454=CARTESIAN_POINT('Ctrl Pts',(1.42589267152236,-2.52108564005781,5.20771011688467));
#13455=CARTESIAN_POINT('Ctrl Pts',(2.89143425882939,-0.169265005463949,
5.33472743680867));
#13456=CARTESIAN_POINT('Ctrl Pts',(1.71031452850143,2.33749158903385,5.4617447567327));
#13457=CARTESIAN_POINT('Ctrl Pts',(-1.03633389740425,2.704635792172,5.58876207665671));
#13458=CARTESIAN_POINT('Ctrl Pts',(-2.83437876089513,0.596103812262253,
5.71577939658073));
#13459=CARTESIAN_POINT('Ctrl Pts',(-2.03798779964606,-2.05806910566698,
5.84279671650474));
#13460=CARTESIAN_POINT('Ctrl Pts',(0.62386610915731,-2.82839774307856,5.96981403642876));
#13461=CARTESIAN_POINT('Ctrl Pts',(2.7146669865981,-1.00976525345321,6.09683135635278));
#13462=CARTESIAN_POINT('Ctrl Pts',(2.32060967238186,1.73315131008656,6.2238486762768));
#13463=CARTESIAN_POINT('Ctrl Pts',(-0.197607246870416,2.88963563294601,
6.35086599620081));
#13464=CARTESIAN_POINT('Ctrl Pts',(-2.53494526328089,1.40110500226672,6.47788331612483));
#13465=CARTESIAN_POINT('Ctrl Pts',(-2.5519325574986,-1.36992077770418,6.60490063604884));
#13466=CARTESIAN_POINT('Ctrl Pts',(-0.233019886320138,-2.88699574779499,
6.73191795597286));
#13467=CARTESIAN_POINT('Ctrl Pts',(2.29918648762192,-1.76147217132255,6.85893527589687));
#13468=CARTESIAN_POINT('Ctrl Pts',(2.72684287214744,0.976407018525444,6.98595259582089));
#13469=CARTESIAN_POINT('Ctrl Pts',(0.658495923052897,2.82053644446047,7.11296991574491));
#13470=CARTESIAN_POINT('Ctrl Pts',(-2.01260230148307,2.08290054761913,7.23998723566893));
#13471=CARTESIAN_POINT('Ctrl Pts',(-2.84147407980028,-0.561308978219811,
7.36700455559294));
#13472=CARTESIAN_POINT('Ctrl Pts',(-1.06941536519506,-2.69172686056585,
7.49402187551696));
#13473=CARTESIAN_POINT('Ctrl Pts',(1.68152788427493,-2.35828469223139,7.62103919544097));
#13474=CARTESIAN_POINT('Ctrl Pts',(2.89329216322361,0.133802740763723,7.74805651536499));
#13475=CARTESIAN_POINT('Ctrl Pts',(1.45669450012326,2.50341443802613,7.87507383528901));
#13476=CARTESIAN_POINT('Ctrl Pts',(-1.31328190859961,2.58153701188885,8.00209115521302));
#13477=CARTESIAN_POINT('Ctrl Pts',(-2.88115164101586,0.296661316451321,
8.12910847513705));
#13478=CARTESIAN_POINT('Ctrl Pts',(-1.81177220367078,-2.25976197799966,
8.25612579506105));
#13479=CARTESIAN_POINT('Ctrl Pts',(0.91600475496642,-2.74772233023752,8.38314311498508));
#13480=CARTESIAN_POINT('Ctrl Pts',(2.80532088941706,-0.72056743099262,8.51016043490908));
#13481=CARTESIAN_POINT('Ctrl Pts',(2.12679919082649,1.96615561874099,8.63717775483311));
#13482=CARTESIAN_POINT('Ctrl Pts',(-0.498478561978086,2.8531669839768,8.76419507475712));
#13483=CARTESIAN_POINT('Ctrl Pts',(-2.66747620963103,1.12854480915004,8.89121239468115));
#13484=CARTESIAN_POINT('Ctrl Pts',(-2.39481153064322,-1.62908577057971,
9.01822971460514));
#13485=CARTESIAN_POINT('Ctrl Pts',(0.0699330899254719,-2.89554003221169,
9.14524703452918));
#13486=CARTESIAN_POINT('Ctrl Pts',(2.47066477180699,-1.51157477504718,9.27226435445317));
#13487=CARTESIAN_POINT('Ctrl Pts',(2.60988458966556,1.25600364005573,9.39928167437721));
#13488=CARTESIAN_POINT('Ctrl Pts',(0.360158310663512,2.87390478382062,9.52629899430121));
#13489=CARTESIAN_POINT('Ctrl Pts',(-2.21923725483436,1.86119013589752,9.65331631422524));
#13490=CARTESIAN_POINT('Ctrl Pts',(-2.76726400083069,-0.855156514863526,
9.78033363414925));
#13491=CARTESIAN_POINT('Ctrl Pts',(-0.782288115237663,-2.78873950378391,
9.90735095407327));
#13492=CARTESIAN_POINT('Ctrl Pts',(1.91875167100355,-2.16966235627301,10.0343682739973));
#13493=CARTESIAN_POINT('Ctrl Pts',(2.86347076266717,0.435405450766662,10.1613855939213));
#13494=CARTESIAN_POINT('Ctrl Pts',(1.18712479688131,2.64192684074267,10.2884029138453));
#13495=CARTESIAN_POINT('Ctrl Pts',(-1.57585050156767,2.43017240374339,10.4154202337693));
#13496=CARTESIAN_POINT('Ctrl Pts',(-2.89637814548709,-0.00602939066377948,
10.5424375536933));
#13497=CARTESIAN_POINT('Ctrl Pts',(-1.56571910740061,-2.43671220950026,
10.6694548736174));
#13498=CARTESIAN_POINT('Ctrl Pts',(1.19811385922502,-2.63696148920304,10.7964721935414));
#13499=CARTESIAN_POINT('Ctrl Pts',(2.86525870449697,-0.423479954084387,
10.9234895134654));
#13500=CARTESIAN_POINT('Ctrl Pts',(1.9097019078235,2.17763204845591,11.0505068333894));
#13501=CARTESIAN_POINT('Ctrl Pts',(-0.793891923486379,2.78545836964585,
11.1775241533134));
#13502=CARTESIAN_POINT('Ctrl Pts',(-2.77080036056394,0.843627925750284,
11.3045414732374));
#13503=CARTESIAN_POINT('Ctrl Pts',(-2.21146917510807,-1.87041353789847,
11.4315587931615));
#13504=CARTESIAN_POINT('Ctrl Pts',(0.372120353081287,-2.87238039925594,
11.5585761130855));
#13505=CARTESIAN_POINT('Ctrl Pts',(2.61509119315851,-1.24512680746655,11.6855934330095));
#13506=CARTESIAN_POINT('Ctrl Pts',(2.46435009533307,1.52184799597032,11.8126107529335));
#13507=CARTESIAN_POINT('Ctrl Pts',(0.0578772441359576,2.89580609499639,
11.9396280728575));
#13508=CARTESIAN_POINT('Ctrl Pts',(-2.40157328163847,1.61910113585509,12.0666453927815));
#13509=CARTESIAN_POINT('Ctrl Pts',(-2.66275452753254,-1.13964075098778,
12.1936627127056));
#13510=CARTESIAN_POINT('Ctrl Pts',(-0.48659541721494,-2.85521761257394,
12.3206800326296));
#13511=CARTESIAN_POINT('Ctrl Pts',(2.13496661525059,-1.95728390045299,12.4476973525536));
#13512=CARTESIAN_POINT('Ctrl Pts',(2.80229657836465,0.732240808814111,12.5747146724776));
#13513=CARTESIAN_POINT('Ctrl Pts',(0.90455699792931,2.75151219381346,12.7017319924016));
#13514=CARTESIAN_POINT('Ctrl Pts',(-1.82116475388173,2.25219929278605,12.8287493123256));
#13515=CARTESIAN_POINT('Ctrl Pts',(-2.8798915558956,-0.308654080627915,
12.9557666322497));
#13516=CARTESIAN_POINT('Ctrl Pts',(-1.30252260138397,-2.58698233238864,
13.0827839521737));
#13517=CARTESIAN_POINT('Ctrl Pts',(1.46710454606473,-2.49732796527072,13.2098012720977));
#13518=CARTESIAN_POINT('Ctrl Pts',(2.89382415925463,-0.12175570015915,13.3368185920217));
#13519=CARTESIAN_POINT('Ctrl Pts',(1.67169487022615,2.36526509636163,13.4638359119457));
#13520=CARTESIAN_POINT('Ctrl Pts',(-1.08061278422976,2.68725114676061,13.5908532318697));
#13521=CARTESIAN_POINT('Ctrl Pts',(-2.84378639677227,0.549473970939458,
13.7178705517938));
#13522=CARTESIAN_POINT('Ctrl Pts',(-2.00391294747326,-2.09126172779881,
13.8448878717178));
#13523=CARTESIAN_POINT('Ctrl Pts',(0.670233187013017,-2.81777042894438,
13.9719051916418));
#13524=CARTESIAN_POINT('Ctrl Pts',(2.73088439438974,-0.965045667150298,
14.0989225115658));
#13525=CARTESIAN_POINT('Ctrl Pts',(2.29183287897636,1.77102929677913,14.2259398314898));
#13526=CARTESIAN_POINT('Ctrl Pts',(-0.245037533321299,2.88600057561859,
14.3529571514138));
#13527=CARTESIAN_POINT('Ctrl Pts',(-2.55761394383426,1.35928423426138,14.4799744713379));
#13528=CARTESIAN_POINT('Ctrl Pts',(-2.52908995757369,-1.41164680487256,
14.6069917912619));
#13529=CARTESIAN_POINT('Ctrl Pts',(-0.185574876810634,-2.8904333032097,
14.7340091111859));
#13530=CARTESIAN_POINT('Ctrl Pts',(2.32780533108778,-1.72347470412719,14.8610264311099));
#13531=CARTESIAN_POINT('Ctrl Pts',(2.71043942018326,1.02105869798148,14.9880437510339));
#13532=CARTESIAN_POINT('Ctrl Pts',(0.612085001486641,2.83097062262435,15.1150610709579));
#13533=CARTESIAN_POINT('Ctrl Pts',(-2.04653866476156,2.04956634653356,15.242078390882));
#13534=CARTESIAN_POINT('Ctrl Pts',(-2.83187238760927,-0.607899247822501,
15.369095710806));
#13535=CARTESIAN_POINT('Ctrl Pts',(-1.02506448320845,-2.70892700537901,
15.49611303073));
#13536=CARTESIAN_POINT('Ctrl Pts',(1.72003157611233,-2.33035063721826,15.623130350654));
#13537=CARTESIAN_POINT('Ctrl Pts',(2.89070448411775,0.181301684240713,15.750147670578));
#13538=CARTESIAN_POINT('Ctrl Pts',(1.41538407048151,2.52700032612467,15.877164990502));
#13539=CARTESIAN_POINT('Ctrl Pts',(-1.3555017731835,2.55962060823541,16.004182310426));
#13540=CARTESIAN_POINT('Ctrl Pts',(-2.88563517777252,0.249303702356721,
16.1311996303501));
#13541=CARTESIAN_POINT('Ctrl Pts',(-1.77441542743651,-2.28921222390636,
16.2582169502741));
#13542=CARTESIAN_POINT('Ctrl Pts',(0.961007487425978,-2.73230805809268,
16.3852342701981));
#13543=CARTESIAN_POINT('Ctrl Pts',(2.81677652976444,-0.67439802533461,16.5122515901221));
#13544=CARTESIAN_POINT('Ctrl Pts',(2.09422187029827,2.00081920052048,16.6392689100461));
#13545=CARTESIAN_POINT('Ctrl Pts',(-0.545269339856637,2.84459558851857,
16.7662862299701));
#13546=CARTESIAN_POINT('Ctrl Pts',(-2.68565071720656,1.08458422465704,16.8933035498942));
#13547=CARTESIAN_POINT('Ctrl Pts',(-2.36773381431579,-1.66819642121442,
17.0203208698181));
#13548=CARTESIAN_POINT('Ctrl Pts',(0.117477564550026,-2.89400099119444,
17.1473381897422));
#13549=CARTESIAN_POINT('Ctrl Pts',(2.49515638415566,-1.47079479663692,17.2743555096662));
#13550=CARTESIAN_POINT('Ctrl Pts',(2.58890505275436,1.29869678640933,17.4013728295902));
#13551=CARTESIAN_POINT('Ctrl Pts',(0.312911149053036,2.87943211901328,17.5283901495142));
#13552=CARTESIAN_POINT('Ctrl Pts',(-2.24950456469862,1.82449223857137,17.6554074694383));
#13553=CARTESIAN_POINT('Ctrl Pts',(-2.75284641327388,-0.900488389781994,
17.7824247893623));
#13554=CARTESIAN_POINT('Ctrl Pts',(-0.73638270405237,-2.80121102889081,
17.9094421092863));
#13555=CARTESIAN_POINT('Ctrl Pts',(1.95412559457642,-2.13785777726871,18.0364594292103));
#13556=CARTESIAN_POINT('Ctrl Pts',(2.85593383710927,0.482373955828185,18.1634767491343));
#13557=CARTESIAN_POINT('Ctrl Pts',(1.14357591303448,2.66106686243213,18.2904940690583));
#13558=CARTESIAN_POINT('Ctrl Pts',(-1.61554906914139,2.40396420946806,18.4175113889823));
#13559=CARTESIAN_POINT('Ctrl Pts',(-2.89588849187353,-0.0535962483896853,
18.5445287089064));
#13560=CARTESIAN_POINT('Ctrl Pts',(-1.52548943482816,-2.46209762183279,
18.6715460288304));
#13561=CARTESIAN_POINT('Ctrl Pts',(1.2412595012752,-2.61692903337118,18.7985633487544));
#13562=CARTESIAN_POINT('Ctrl Pts',(2.87182714702407,-0.376366248251089,
18.9255806686784));
#13563=CARTESIAN_POINT('Ctrl Pts',(1.87368075656313,2.20870168598933,19.0525979886024));
#13564=CARTESIAN_POINT('Ctrl Pts',(-0.839530870069032,2.77204448618851,
19.1796153085265));
#13565=CARTESIAN_POINT('Ctrl Pts',(-2.78428169840113,0.798008859070859,
19.3066326284505));
#13566=CARTESIAN_POINT('Ctrl Pts',(-2.18045282236851,-1.90648058071206,
19.4336499483745));
#13567=CARTESIAN_POINT('Ctrl Pts',(0.41924371770261,-2.86588161311206,19.5606672682985));
#13568=CARTESIAN_POINT('Ctrl Pts',(2.63518741023224,-1.2020108269732,19.6876845882225));
#13569=CARTESIAN_POINT('Ctrl Pts',(2.43902418313076,1.56211515238478,19.8147019081465));
#13570=CARTESIAN_POINT('Ctrl Pts',(0.0103111622528317,2.89636606718479,
19.9417192280705));
#13571=CARTESIAN_POINT('Ctrl Pts',(-2.42784013452314,1.57944135579879,20.0687365479946));
#13572=CARTESIAN_POINT('Ctrl Pts',(-2.64367890600989,-1.18321788235451,
20.1957538679186));
#13573=CARTESIAN_POINT('Ctrl Pts',(-0.439638105477045,-2.86282396444784,
20.3227711878426));
#13574=CARTESIAN_POINT('Ctrl Pts',(2.16682345353623,-1.92195703292896,20.4497885077666));
#13575=CARTESIAN_POINT('Ctrl Pts',(2.78989292983982,0.778164606764122,20.5768058276906));
#13576=CARTESIAN_POINT('Ctrl Pts',(0.859246486382724,2.76599678069832,20.7038231476147));
#13577=CARTESIAN_POINT('Ctrl Pts',(-1.85790735593631,2.22198626729555,20.8308404675387));
#13578=CARTESIAN_POINT('Ctrl Pts',(-2.87443407321436,-0.355909361805081,
20.9578577874627));
#13579=CARTESIAN_POINT('Ctrl Pts',(-1.25986051623017,-2.60802496054242,
21.0848751073868));
#13580=CARTESIAN_POINT('Ctrl Pts',(1.50792068648154,-2.47289666566219,21.2118924273106));
#13581=CARTESIAN_POINT('Ctrl Pts',(2.89543348443989,-0.0742135525751324,
21.3389097472348));
#13582=CARTESIAN_POINT('Ctrl Pts',(1.63262429222479,2.3924006010089,21.4659270671587));
#13583=CARTESIAN_POINT('Ctrl Pts',(-1.12460018907184,2.66914164732104,21.5929443870828));
#13584=CARTESIAN_POINT('Ctrl Pts',(-2.85242695349848,0.502695914710937,
21.7199617070067));
#13585=CARTESIAN_POINT('Ctrl Pts',(-1.96929756557384,-2.12389025520565,
21.8469790269308));
#13586=CARTESIAN_POINT('Ctrl Pts',(0.716419481622734,-2.80638305708953,
21.9739963468548));
#13587=CARTESIAN_POINT('Ctrl Pts',(2.74636517004355,-0.920065765881881,
22.1010136667789));
#13588=CARTESIAN_POINT('Ctrl Pts',(2.26243790611172,1.80842955915543,22.2280309867028));
#13589=CARTESIAN_POINT('Ctrl Pts',(-0.292401753364768,2.88158707253183,
22.3550483066269));
#13590=CARTESIAN_POINT('Ctrl Pts',(-2.57959268171739,1.3170967791333,22.4820656265509));
#13591=CARTESIAN_POINT('Ctrl Pts',(-2.50556527268738,-1.45299198800726,
22.6090829464749));
#13592=CARTESIAN_POINT('Ctrl Pts',(-0.138079606205935,-2.89309132941754,
22.7361002663989));
#13593=CARTESIAN_POINT('Ctrl Pts',(2.35579588699587,-1.68501209994816,22.8631175863229));
#13594=CARTESIAN_POINT('Ctrl Pts',(2.69330560074701,1.06543448281075,22.9901349062469));
#13595=CARTESIAN_POINT('Ctrl Pts',(0.565507564442487,2.84064208642623,23.117152226171));
#13596=CARTESIAN_POINT('Ctrl Pts',(-2.07992030745382,2.01567757201905,23.2441695460949));
#13597=CARTESIAN_POINT('Ctrl Pts',(-2.82151195628706,-0.65432225437952,
23.371186866019));
#13598=CARTESIAN_POINT('Ctrl Pts',(-0.980427340272484,-2.72540271416528,
23.498204185943));
#13599=CARTESIAN_POINT('Ctrl Pts',(1.75805271638312,-2.30177606424313,23.6252215058671));
#13600=CARTESIAN_POINT('Ctrl Pts',(2.88737248580153,0.228728994565927,23.752238825791));
#13601=CARTESIAN_POINT('Ctrl Pts',(1.37362440389478,2.54994787792699,23.8792561457151));
#13602=CARTESIAN_POINT('Ctrl Pts',(-1.39722752465262,2.53693131462652,24.0062734656391));
#13603=CARTESIAN_POINT('Ctrl Pts',(-2.88958510439483,0.202035941526333,
24.1332907855631));
#13604=CARTESIAN_POINT('Ctrl Pts',(-1.73611351559699,-2.31834451256072,
24.2603081054871));
#13605=CARTESIAN_POINT('Ctrl Pts',(1.0048596332272,-2.71558362271932,24.3873254254111));
#13606=CARTESIAN_POINT('Ctrl Pts',(2.82919456675196,-0.629161302687018,
24.5143427453351));
#13607=CARTESIAN_POINT('Ctrl Pts',(2.05758802371498,2.03726316769148,24.6413600652592));
#13608=CARTESIAN_POINT('Ctrl Pts',(0.296877711348344,2.56531103767014,24.7260382785418));
#13609=CARTESIAN_POINT('Ctrl Pts',(-0.500790878576573,2.39878276338949,
24.7683773851832));
#13610=CARTESIAN_POINT('Ctrl Pts',(-2.45061074833635,-0.00223305219117096,
23.342172503788));
#13611=CARTESIAN_POINT('Ctrl Pts',(-2.45232391003785,-0.188294688285105,
23.351843957865));
#13612=CARTESIAN_POINT('Ctrl Pts',(-2.43292514735263,-0.37400280173149,
23.361515411942));
#13613=CARTESIAN_POINT('Ctrl Pts',(-2.39106591214575,-0.55450235994407,
23.371186866019));
#13614=CARTESIAN_POINT('Ctrl Pts',(-2.20781708428219,-1.34468240764144,
23.4135259726603));
#13615=CARTESIAN_POINT('Ctrl Pts',(-1.59412221227735,-2.03504256090335,
23.4558650793016));
#13616=CARTESIAN_POINT('Ctrl Pts',(-0.830861433498997,-2.30961819588062,
23.498204185943));
#13617=CARTESIAN_POINT('Ctrl Pts',(-0.0676006547206245,-2.58419383085789,
23.5405432925843));
#13618=CARTESIAN_POINT('Ctrl Pts',(0.84522603083126,-2.44298494755051,23.5828823992257));
#13619=CARTESIAN_POINT('Ctrl Pts',(1.48985933517694,-1.95062966276197,23.625221505867));
#13620=CARTESIAN_POINT('Ctrl Pts',(2.13449263952259,-1.45827437797344,23.6675606125084));
#13621=CARTESIAN_POINT('Ctrl Pts',(2.51093256266206,-0.614772691703766,
23.7098997191497));
#13622=CARTESIAN_POINT('Ctrl Pts',(2.44686117724734,0.193847965324576,23.752238825791));
#13623=CARTESIAN_POINT('Ctrl Pts',(2.38278979183262,1.00246862235294,23.7945779324324));
#13624=CARTESIAN_POINT('Ctrl Pts',(1.87820709786369,1.77620825013998,23.8369170390737));
#13625=CARTESIAN_POINT('Ctrl Pts',(1.16410709612132,2.16090863681675,23.8792561457151));
#13626=CARTESIAN_POINT('Ctrl Pts',(0.450007094378972,2.5456090234935,23.9215952523564));
#13627=CARTESIAN_POINT('Ctrl Pts',(-0.473610215136808,2.54127016906001,
23.9639343589977));
#13628=CARTESIAN_POINT('Ctrl Pts',(-1.18414513318507,2.14995151299324,24.0062734656391));
#13629=CARTESIAN_POINT('Ctrl Pts',(-1.42595437674378,2.01677794782373,24.0206823104261));
#13630=CARTESIAN_POINT('Ctrl Pts',(-1.6430849072501,1.83878527106171,24.035091155213));
#13631=CARTESIAN_POINT('Ctrl Pts',(-1.82655445601566,1.63000783787709,24.0495));
#13632=CARTESIAN_POINT('Ctrl Pts',(-1.1628446574583,-1.62479335886121,-9.36750677027476E-17));
#13633=CARTESIAN_POINT('Ctrl Pts',(-1.20471710970498,-1.6016342897335,-9.84898357583373E-17));
#13634=CARTESIAN_POINT('Ctrl Pts',(-1.24562209910426,-1.57691188235754,
-1.47679554909033E-16));
#13635=CARTESIAN_POINT('Ctrl Pts',(-1.2854610045556,-1.55064518989967,-1.64798730217797E-16));
#13636=CARTESIAN_POINT('Ctrl Pts',(-1.34528284791422,-1.51120329399511,
-1.79293118691912E-16));
#13637=CARTESIAN_POINT('Ctrl Pts',(-1.40270227022668,-1.46828195181486,
-2.83591590275869E-17));
#13638=CARTESIAN_POINT('Ctrl Pts',(-1.45763752553965,-1.42222527204903,
7.28583859910259E-17));
#13639=CARTESIAN_POINT('Ctrl Pts',(-1.48804755094941,-1.39673008150174,
1.28888490855271E-16));
#13640=CARTESIAN_POINT('Ctrl Pts',(-1.51769605100349,-1.37027322214852,
-3.8021251132136E-16));
#13641=CARTESIAN_POINT('Ctrl Pts',(-1.54656641082207,-1.34290698199124,
-3.67761376907083E-16));
#13642=CARTESIAN_POINT('Ctrl Pts',(-1.55885125016836,-1.33126217167516,
-3.62463203038807E-16));
#13643=CARTESIAN_POINT('Ctrl Pts',(-1.57099516808733,-1.31945265506341,
-7.47886777659616E-16));
#13644=CARTESIAN_POINT('Ctrl Pts',(-1.58299675523336,-1.30748225159357,
-7.49400541621981E-16));
#13645=CARTESIAN_POINT('Ctrl Pts',(-1.59344058720201,-1.29706555579204,
-7.50717825433759E-16));
#13646=CARTESIAN_POINT('Ctrl Pts',(-1.60377038195195,-1.28653323791471,
-4.4644076430482E-16));
#13647=CARTESIAN_POINT('Ctrl Pts',(-1.61398372332283,-1.27589015849519,
-4.57966997657877E-16));
#13648=CARTESIAN_POINT('Ctrl Pts',(-1.66603051092346,-1.22165344263028,
-5.16704231377666E-16));
#13649=CARTESIAN_POINT('Ctrl Pts',(-1.71507034489567,-1.16452912219097,
-1.54529368863996E-16));
#13650=CARTESIAN_POINT('Ctrl Pts',(-1.76101022097129,-1.10489021342489,
-2.35922392732846E-16));
#13651=CARTESIAN_POINT('Ctrl Pts',(-1.79846063902999,-1.05627227500952,
-3.02274395205222E-16));
#13652=CARTESIAN_POINT('Ctrl Pts',(-1.83385070502955,-1.00598204477662,
-3.07161165321323E-16));
#13653=CARTESIAN_POINT('Ctrl Pts',(-1.86711657018502,-0.954199806015946,
-2.42861286636753E-16));
#13654=CARTESIAN_POINT('Ctrl Pts',(-1.88036622467999,-0.933575157615885,
-2.17250914783866E-16));
#13655=CARTESIAN_POINT('Ctrl Pts',(-1.89327874453011,-0.912713625458099,
-5.33570700749379E-16));
#13656=CARTESIAN_POINT('Ctrl Pts',(-1.90584944825313,-0.891625897229556,
-5.68989300120393E-16));
#13657=CARTESIAN_POINT('Ctrl Pts',(-1.91458650894537,-0.876969218856263,
-5.93606414576128E-16));
#13658=CARTESIAN_POINT('Ctrl Pts',(-1.92315966451329,-0.862200842946139,
-7.8088903438659E-16));
#13659=CARTESIAN_POINT('Ctrl Pts',(-1.93155555809178,-0.847345668566372,
-7.63278329429795E-16));
#13660=CARTESIAN_POINT('Ctrl Pts',(-1.96982617330085,-0.779632011022089,
-6.83004263702097E-16));
#13661=CARTESIAN_POINT('Ctrl Pts',(-2.00447064936929,-0.710029521402437,
-3.10624695463674E-16));
#13662=CARTESIAN_POINT('Ctrl Pts',(-2.03539350763164,-0.638916805331437,
-3.33066907387547E-16));
#13663=CARTESIAN_POINT('Ctrl Pts',(-2.06690570609391,-0.566448794677043,
-3.55936831961706E-16));
#13664=CARTESIAN_POINT('Ctrl Pts',(-2.09455376203166,-0.492411684095305,
-4.04707542421149E-16));
#13665=CARTESIAN_POINT('Ctrl Pts',(-2.1182014521557,-0.417165542608831,
-3.05311331771918E-16));
#13666=CARTESIAN_POINT('Ctrl Pts',(-2.13556664588564,-0.361910089856805,
-2.32321773599738E-16));
#13667=CARTESIAN_POINT('Ctrl Pts',(-2.1507739922553,-0.306001765547992,
-4.24436518415042E-16));
#13668=CARTESIAN_POINT('Ctrl Pts',(-2.16375453913393,-0.249573411217413,
-3.7470027081099E-16));
#13669=CARTESIAN_POINT('Ctrl Pts',(-2.17348994929291,-0.20725214546948,
-3.37398085107951E-16));
#13670=CARTESIAN_POINT('Ctrl Pts',(-2.18197253287921,-0.164638180799305,
-2.06086771920563E-16));
#13671=CARTESIAN_POINT('Ctrl Pts',(-2.18916775342387,-0.12178566500651,
-1.80411241501588E-16));
#13672=CARTESIAN_POINT('Ctrl Pts',(-2.1911236200848,-0.110137126027669,
-1.73431898250564E-16));
#13673=CARTESIAN_POINT('Ctrl Pts',(-2.1929844738391,-0.0984700252994666,
-5.62880969893907E-16));
#13674=CARTESIAN_POINT('Ctrl Pts',(-2.19474912408356,-0.086788305589102,
-5.55111512312578E-16));
#13675=CARTESIAN_POINT('Ctrl Pts',(-2.20686349029083,-0.00659301989632839,
-5.01773999869121E-16));
#13676=CARTESIAN_POINT('Ctrl Pts',(-2.21439544409116,0.0739404855027051,
-3.28643147674851E-16));
#13677=CARTESIAN_POINT('Ctrl Pts',(-2.21721959193008,0.154432844333648,
-4.16333634234434E-16));
#13678=CARTESIAN_POINT('Ctrl Pts',(-2.21852422549391,0.19161681590748,-4.56842827987537E-16));
#13679=CARTESIAN_POINT('Ctrl Pts',(-2.21882361008786,0.228792448646571,
-4.07756221638516E-16));
#13680=CARTESIAN_POINT('Ctrl Pts',(-2.21810211756152,0.26592419994786,-4.44089209850063E-16));
#13681=CARTESIAN_POINT('Ctrl Pts',(-2.21659417953099,0.343530520017813,
-5.19153256660931E-16));
#13682=CARTESIAN_POINT('Ctrl Pts',(-2.21063041400095,0.420944765509284,
-3.26957043112244E-16));
#13683=CARTESIAN_POINT('Ctrl Pts',(-2.20044401683584,0.497916376546012,
-3.33066907387547E-16));
#13684=CARTESIAN_POINT('Ctrl Pts',(-2.19004534119325,0.576492030320754,
-3.39304097611847E-16));
#13685=CARTESIAN_POINT('Ctrl Pts',(-2.17524608828998,0.654607181552501,
-1.21848361755045E-16));
#13686=CARTESIAN_POINT('Ctrl Pts',(-2.15624041704135,0.731997413041652,
-1.38777878078145E-16));
#13687=CARTESIAN_POINT('Ctrl Pts',(-2.1530491332955,0.744992175742075,-1.4162055011851E-16));
#13688=CARTESIAN_POINT('Ctrl Pts',(-2.14973861875141,0.757968425128774,
-2.74413855480096E-16));
#13689=CARTESIAN_POINT('Ctrl Pts',(-2.14631128719358,0.770918735048493,
-2.77555756156289E-16));
#13690=CARTESIAN_POINT('Ctrl Pts',(-2.1256470659196,0.848999324928004,-2.96499044746354E-16));
#13691=CARTESIAN_POINT('Ctrl Pts',(-2.100810416393,0.925878399842031,-5.72875657946036E-16));
#13692=CARTESIAN_POINT('Ctrl Pts',(-2.07208060636904,1.00128708760705,-4.71844785465692E-16));
#13693=CARTESIAN_POINT('Ctrl Pts',(-2.04275443716757,1.07826107159141,-3.68716764136624E-16));
#13694=CARTESIAN_POINT('Ctrl Pts',(-2.00937162894103,1.15370380486668,-4.21201560705881E-16));
#13695=CARTESIAN_POINT('Ctrl Pts',(-1.97217365940411,1.22733228755951,-4.71844785465692E-16));
#13696=CARTESIAN_POINT('Ctrl Pts',(-1.93463599538849,1.301633150744,-5.22950487722222E-16));
#13697=CARTESIAN_POINT('Ctrl Pts',(-1.89321286071335,1.37408738698341,-2.7977493126578E-16));
#13698=CARTESIAN_POINT('Ctrl Pts',(-1.84810028796748,1.44439403673038,-1.94289029309402E-16));
#13699=CARTESIAN_POINT('Ctrl Pts',(-1.82057954912994,1.48728431827401,-1.42138707595646E-16));
#13700=CARTESIAN_POINT('Ctrl Pts',(-1.79168476892488,1.52937510966431,-4.41214674814833E-16));
#13701=CARTESIAN_POINT('Ctrl Pts',(-1.7614518395478,1.57059399934622,-4.9960036108132E-16));
#13702=CARTESIAN_POINT('Ctrl Pts',(-1.75330578858498,1.58170014032886,-5.15331975107013E-16));
#13703=CARTESIAN_POINT('Ctrl Pts',(-1.74506709433522,1.59273671109622,-3.76832932046581E-17));
#13704=CARTESIAN_POINT('Ctrl Pts',(-1.73674048345306,1.60369766068764,-2.77555756156289E-17));
#13705=CARTESIAN_POINT('Ctrl Pts',(-1.68479340016487,1.67207954731607,3.41803043909498E-17));
#13706=CARTESIAN_POINT('Ctrl Pts',(-1.62938511172315,1.73757860209274,-5.37469459706135E-16));
#13707=CARTESIAN_POINT('Ctrl Pts',(-1.57077056839118,1.79989799981718,-4.44089209850063E-16));
#13708=CARTESIAN_POINT('Ctrl Pts',(-1.51209289484641,1.86228451803112,-3.50608385721631E-16));
#13709=CARTESIAN_POINT('Ctrl Pts',(-1.45020161829715,1.92148546079072,4.07133896698368E-17));
#13710=CARTESIAN_POINT('Ctrl Pts',(-1.38530359897227,1.97718510495395,1.94289029309402E-16));
#13711=CARTESIAN_POINT('Ctrl Pts',(-1.32180103027288,2.03168708385566,3.44562453802459E-16));
#13712=CARTESIAN_POINT('Ctrl Pts',(-1.25541907256516,2.08283749691017,-1.49241330947029E-16));
#13713=CARTESIAN_POINT('Ctrl Pts',(-1.18631234985499,2.13031087324772,-2.22044604925031E-16));
#13714=CARTESIAN_POINT('Ctrl Pts',(-1.14998501104135,2.15526620840483,-2.60315110265489E-16));
#13715=CARTESIAN_POINT('Ctrl Pts',(-1.11290413210694,2.1792049027253,-6.37841755674301E-18));
#13716=CARTESIAN_POINT('Ctrl Pts',(-1.07508846035128,2.20207516956609,0.));
#13717=CARTESIAN_POINT('Origin',(0.,0.,0.));
#13718=CARTESIAN_POINT('Origin',(-1.15470053837925,-2.,-5.));
#13719=CARTESIAN_POINT('',(-1.15470053837925,-2.,-5.));
#13720=CARTESIAN_POINT('',(1.15470053837925,-2.,-5.));
#13721=CARTESIAN_POINT('',(-0.577350269189627,-2.,-5.));
#13722=CARTESIAN_POINT('',(-1.15470053837925,-2.,-2.));
#13723=CARTESIAN_POINT('',(-1.15470053837925,-2.,-5.));
#13724=CARTESIAN_POINT('',(1.15470053837925,-2.,-2.));
#13725=CARTESIAN_POINT('',(-1.15470053837925,-2.,-2.));
#13726=CARTESIAN_POINT('',(1.15470053837925,-2.,-5.));
#13727=CARTESIAN_POINT('Origin',(-2.3094010767585,2.82820063659975E-16,
-5.));
#13728=CARTESIAN_POINT('',(-2.3094010767585,2.82820063659975E-16,-5.));
#13729=CARTESIAN_POINT('',(-2.02072594216369,-0.5,-5.));
#13730=CARTESIAN_POINT('',(-2.3094010767585,2.77555756156289E-16,-2.));
#13731=CARTESIAN_POINT('',(-2.3094010767585,2.82820063659975E-16,-5.));
#13732=CARTESIAN_POINT('',(-2.3094010767585,2.82820063659975E-16,-2.));
#13733=CARTESIAN_POINT('Origin',(-1.15470053837925,2.,-5.));
#13734=CARTESIAN_POINT('',(-1.15470053837925,2.,-5.));
#13735=CARTESIAN_POINT('',(-1.44337567297406,1.5,-5.));
#13736=CARTESIAN_POINT('',(-1.15470053837925,2.,-2.));
#13737=CARTESIAN_POINT('',(-1.15470053837925,2.,-5.));
#13738=CARTESIAN_POINT('',(-1.15470053837925,2.,-2.));
#13739=CARTESIAN_POINT('Origin',(1.15470053837925,2.,-5.));
#13740=CARTESIAN_POINT('',(1.15470053837925,2.,-5.));
#13741=CARTESIAN_POINT('',(0.577350269189626,2.,-5.));
#13742=CARTESIAN_POINT('',(1.15470053837925,2.,-2.));
#13743=CARTESIAN_POINT('',(1.15470053837925,2.,-5.));
#13744=CARTESIAN_POINT('',(1.15470053837925,2.,-2.));
#13745=CARTESIAN_POINT('Origin',(2.3094010767585,0.,-5.));
#13746=CARTESIAN_POINT('',(2.3094010767585,0.,-5.));
#13747=CARTESIAN_POINT('',(2.02072594216369,0.5,-5.));
#13748=CARTESIAN_POINT('',(2.3094010767585,0.,-2.));
#13749=CARTESIAN_POINT('',(2.3094010767585,0.,-5.));
#13750=CARTESIAN_POINT('',(2.3094010767585,0.,-2.));
#13751=CARTESIAN_POINT('Origin',(1.15470053837925,-2.,-5.));
#13752=CARTESIAN_POINT('',(1.44337567297406,-1.5,-5.));
#13753=CARTESIAN_POINT('',(1.15470053837925,-2.,-2.));
#13754=CARTESIAN_POINT('Origin',(0.,0.,-2.));
#13755=CARTESIAN_POINT('Origin',(0.,0.,0.));
#13756=CARTESIAN_POINT('',(-4.,-4.89858719658941E-16,0.));
#13757=CARTESIAN_POINT('Origin',(0.,0.,0.));
#13758=CARTESIAN_POINT('Origin',(0.,0.,-5.));
#13759=CARTESIAN_POINT('',(-4.,-4.89858719658941E-16,-5.));
#13760=CARTESIAN_POINT('',(-4.,-4.89858719658941E-16,-5.));
#13761=CARTESIAN_POINT('Origin',(0.,0.,-5.));
#13762=CARTESIAN_POINT('Origin',(0.,0.,-5.));
#13763=CARTESIAN_POINT('Origin',(0.,0.,25.));
#13764=CARTESIAN_POINT('',(0.,0.,0.));
#13765=CARTESIAN_POINT('Origin',(0.,0.,0.));
#13766=CARTESIAN_POINT('',(-1.,-1.22464679914735E-16,10.));
#13767=CARTESIAN_POINT('Origin',(0.,0.,10.));
#13768=CARTESIAN_POINT('',(-1.,-1.22464679914735E-16,0.));
#13769=CARTESIAN_POINT('',(-1.,-1.22464679914735E-16,0.));
#13770=CARTESIAN_POINT('Origin',(0.,0.,0.));
#13771=CARTESIAN_POINT('Origin',(0.,0.,10.));
#13772=CARTESIAN_POINT('Origin',(0.,0.,0.));
#13773=CARTESIAN_POINT('',(0.,0.,0.));
#13774=CARTESIAN_POINT('',(0.,0.,0.));
#13775=CARTESIAN_POINT('',(0.,0.,0.));
#13776=CARTESIAN_POINT('',(-14.,-6.,0.));
#13777=CARTESIAN_POINT('',(-14.,-6.,0.));
#13778=CARTESIAN_POINT('',(-5.,0.,-3.));
#13779=CARTESIAN_POINT('',(-14.,6.,0.));
#13780=CARTESIAN_POINT('',(-14.,6.,0.));
#13781=CARTESIAN_POINT('',(-5.,0.,3.));
#13782=CARTESIAN_POINT('',(0.,30.,0.));
#13783=CARTESIAN_POINT('',(0.,-30.,0.));
#13784=UNCERTAINTY_MEASURE_WITH_UNIT(LENGTH_MEASURE(0.01),#13802,
'DISTANCE_ACCURACY_VALUE',
'Maximum model space distance between geometric entities at asserted c
onnectivities');
#13785=UNCERTAINTY_MEASURE_WITH_UNIT(LENGTH_MEASURE(0.01),#13802,
'DISTANCE_ACCURACY_VALUE',
'Maximum model space distance between geometric entities at asserted c
onnectivities');
#13786=UNCERTAINTY_MEASURE_WITH_UNIT(LENGTH_MEASURE(0.01),#13802,
'DISTANCE_ACCURACY_VALUE',
'Maximum model space distance between geometric entities at asserted c
onnectivities');
#13787=UNCERTAINTY_MEASURE_WITH_UNIT(LENGTH_MEASURE(0.01),#13802,
'DISTANCE_ACCURACY_VALUE',
'Maximum model space distance between geometric entities at asserted c
onnectivities');
#13788=UNCERTAINTY_MEASURE_WITH_UNIT(LENGTH_MEASURE(0.01),#13802,
'DISTANCE_ACCURACY_VALUE',
'Maximum model space distance between geometric entities at asserted c
onnectivities');
#13789=UNCERTAINTY_MEASURE_WITH_UNIT(LENGTH_MEASURE(0.01),#13802,
'DISTANCE_ACCURACY_VALUE',
'Maximum model space distance between geometric entities at asserted c
onnectivities');
#13790=UNCERTAINTY_MEASURE_WITH_UNIT(LENGTH_MEASURE(0.01),#13802,
'DISTANCE_ACCURACY_VALUE',
'Maximum model space distance between geometric entities at asserted c
onnectivities');
#13791=UNCERTAINTY_MEASURE_WITH_UNIT(LENGTH_MEASURE(0.01),#13802,
'DISTANCE_ACCURACY_VALUE',
'Maximum model space distance between geometric entities at asserted c
onnectivities');
#13792=UNCERTAINTY_MEASURE_WITH_UNIT(LENGTH_MEASURE(0.01),#13802,
'DISTANCE_ACCURACY_VALUE',
'Maximum model space distance between geometric entities at asserted c
onnectivities');
#13793=(
GEOMETRIC_REPRESENTATION_CONTEXT(3)
GLOBAL_UNCERTAINTY_ASSIGNED_CONTEXT((#13784))
GLOBAL_UNIT_ASSIGNED_CONTEXT((#13802,#13804,#13805))
REPRESENTATION_CONTEXT('','3D')
);
#13794=(
GEOMETRIC_REPRESENTATION_CONTEXT(3)
GLOBAL_UNCERTAINTY_ASSIGNED_CONTEXT((#13785))
GLOBAL_UNIT_ASSIGNED_CONTEXT((#13802,#13804,#13805))
REPRESENTATION_CONTEXT('','3D')
);
#13795=(
GEOMETRIC_REPRESENTATION_CONTEXT(3)
GLOBAL_UNCERTAINTY_ASSIGNED_CONTEXT((#13786))
GLOBAL_UNIT_ASSIGNED_CONTEXT((#13802,#13804,#13805))
REPRESENTATION_CONTEXT('','3D')
);
#13796=(
GEOMETRIC_REPRESENTATION_CONTEXT(3)
GLOBAL_UNCERTAINTY_ASSIGNED_CONTEXT((#13787))
GLOBAL_UNIT_ASSIGNED_CONTEXT((#13802,#13804,#13805))
REPRESENTATION_CONTEXT('','3D')
);
#13797=(
GEOMETRIC_REPRESENTATION_CONTEXT(3)
GLOBAL_UNCERTAINTY_ASSIGNED_CONTEXT((#13788))
GLOBAL_UNIT_ASSIGNED_CONTEXT((#13802,#13804,#13805))
REPRESENTATION_CONTEXT('','3D')
);
#13798=(
GEOMETRIC_REPRESENTATION_CONTEXT(3)
GLOBAL_UNCERTAINTY_ASSIGNED_CONTEXT((#13789))
GLOBAL_UNIT_ASSIGNED_CONTEXT((#13802,#13804,#13805))
REPRESENTATION_CONTEXT('','3D')
);
#13799=(
GEOMETRIC_REPRESENTATION_CONTEXT(3)
GLOBAL_UNCERTAINTY_ASSIGNED_CONTEXT((#13790))
GLOBAL_UNIT_ASSIGNED_CONTEXT((#13802,#13804,#13805))
REPRESENTATION_CONTEXT('','3D')
);
#13800=(
GEOMETRIC_REPRESENTATION_CONTEXT(3)
GLOBAL_UNCERTAINTY_ASSIGNED_CONTEXT((#13791))
GLOBAL_UNIT_ASSIGNED_CONTEXT((#13802,#13804,#13805))
REPRESENTATION_CONTEXT('','3D')
);
#13801=(
GEOMETRIC_REPRESENTATION_CONTEXT(3)
GLOBAL_UNCERTAINTY_ASSIGNED_CONTEXT((#13792))
GLOBAL_UNIT_ASSIGNED_CONTEXT((#13802,#13804,#13805))
REPRESENTATION_CONTEXT('','3D')
);
#13802=(
LENGTH_UNIT()
NAMED_UNIT(*)
SI_UNIT(.MILLI.,.METRE.)
);
#13803=(
LENGTH_UNIT()
NAMED_UNIT(*)
SI_UNIT($,.METRE.)
);
#13804=(
NAMED_UNIT(*)
PLANE_ANGLE_UNIT()
SI_UNIT($,.RADIAN.)
);
#13805=(
NAMED_UNIT(*)
SI_UNIT($,.STERADIAN.)
SOLID_ANGLE_UNIT()
);
#13806=SHAPE_DEFINITION_REPRESENTATION(#13814,#13833);
#13807=SHAPE_DEFINITION_REPRESENTATION(#13815,#13834);
#13808=SHAPE_DEFINITION_REPRESENTATION(#13816,#13835);
#13809=SHAPE_DEFINITION_REPRESENTATION(#13817,#13836);
#13810=SHAPE_DEFINITION_REPRESENTATION(#13818,#13837);
#13811=SHAPE_DEFINITION_REPRESENTATION(#13819,#13838);
#13812=SHAPE_DEFINITION_REPRESENTATION(#13820,#13839);
#13813=SHAPE_DEFINITION_REPRESENTATION(#13821,#13840);
#13814=PRODUCT_DEFINITION_SHAPE('',$,#13842);
#13815=PRODUCT_DEFINITION_SHAPE('',$,#13843);
#13816=PRODUCT_DEFINITION_SHAPE('',$,#13844);
#13817=PRODUCT_DEFINITION_SHAPE('',$,#13845);
#13818=PRODUCT_DEFINITION_SHAPE('',$,#13846);
#13819=PRODUCT_DEFINITION_SHAPE('',$,#13847);
#13820=PRODUCT_DEFINITION_SHAPE('',$,#13848);
#13821=PRODUCT_DEFINITION_SHAPE('',$,#13849);
#13822=PRODUCT_DEFINITION_SHAPE($,$,#44);
#13823=PRODUCT_DEFINITION_SHAPE($,$,#45);
#13824=PRODUCT_DEFINITION_SHAPE($,$,#46);
#13825=PRODUCT_DEFINITION_SHAPE($,$,#47);
#13826=PRODUCT_DEFINITION_SHAPE($,$,#48);
#13827=PRODUCT_DEFINITION_SHAPE($,$,#49);
#13828=PRODUCT_DEFINITION_SHAPE($,$,#50);
#13829=PRODUCT_DEFINITION_SHAPE($,$,#51);
#13830=PRODUCT_DEFINITION_SHAPE($,$,#52);
#13831=PRODUCT_DEFINITION_SHAPE($,$,#53);
#13832=PRODUCT_DEFINITION_SHAPE($,$,#54);
#13833=SHAPE_REPRESENTATION('',(#3767,#4038,#4039),#13793);
#13834=SHAPE_REPRESENTATION('',(#3768,#4029,#4030,#4031,#4032,#4033,#4034,
#4035,#4036,#4037),#13794);
#13835=SHAPE_REPRESENTATION('',(#3769),#13795);
#13836=SHAPE_REPRESENTATION('',(#3802),#13796);
#13837=SHAPE_REPRESENTATION('',(#3925),#13797);
#13838=SHAPE_REPRESENTATION('',(#3932),#13798);
#13839=SHAPE_REPRESENTATION('',(#3941),#13799);
#13840=SHAPE_REPRESENTATION('',(#4023),#13800);
#13841=PRODUCT_DEFINITION_CONTEXT('part definition',#13867,'design');
#13842=PRODUCT_DEFINITION('BR-011','BR-011',#13850,#13841);
#13843=PRODUCT_DEFINITION('Finger module','Finger module',#13851,#13841);
#13844=PRODUCT_DEFINITION('Mounting shoe','Mounting shoe',#13852,#13841);
#13845=PRODUCT_DEFINITION('Flexure finger','Flexure finger',#13853,#13841);
#13846=PRODUCT_DEFINITION('Contact pad','Contact pad',#13854,#13841);
#13847=PRODUCT_DEFINITION('Flat washer M5','Flat washer M5',#13855,#13841);
#13848=PRODUCT_DEFINITION('Socket head cap screw M5x25',
'Socket head cap screw M5x25',#13856,#13841);
#13849=PRODUCT_DEFINITION('Dowel pin','Dowel pin',#13857,#13841);
#13850=PRODUCT_DEFINITION_FORMATION('',$,#13869);
#13851=PRODUCT_DEFINITION_FORMATION('',$,#13870);
#13852=PRODUCT_DEFINITION_FORMATION('',$,#13871);
#13853=PRODUCT_DEFINITION_FORMATION('',$,#13872);
#13854=PRODUCT_DEFINITION_FORMATION('',$,#13873);
#13855=PRODUCT_DEFINITION_FORMATION('',$,#13874);
#13856=PRODUCT_DEFINITION_FORMATION('',$,#13875);
#13857=PRODUCT_DEFINITION_FORMATION('',$,#13876);
#13858=PRODUCT_RELATED_PRODUCT_CATEGORY('BR-011','BR-011',(#13869));
#13859=PRODUCT_RELATED_PRODUCT_CATEGORY('Finger module','Finger module',
(#13870));
#13860=PRODUCT_RELATED_PRODUCT_CATEGORY('Mounting shoe','Mounting shoe',
(#13871));
#13861=PRODUCT_RELATED_PRODUCT_CATEGORY('Flexure finger',
'Flexure finger',(#13872));
#13862=PRODUCT_RELATED_PRODUCT_CATEGORY('Contact pad','Contact pad',(#13873));
#13863=PRODUCT_RELATED_PRODUCT_CATEGORY('Flat washer M5',
'Flat washer M5',(#13874));
#13864=PRODUCT_RELATED_PRODUCT_CATEGORY('Socket head cap screw M5x25',
'Socket head cap screw M5x25',(#13875));
#13865=PRODUCT_RELATED_PRODUCT_CATEGORY('Dowel pin','Dowel pin',(#13876));
#13866=APPLICATION_PROTOCOL_DEFINITION('international standard',
'automotive_design',2009,#13867);
#13867=APPLICATION_CONTEXT(
'Core Data for Automotive Mechanical Design Process');
#13868=PRODUCT_CONTEXT('part definition',#13867,'mechanical');
#13869=PRODUCT('BR-011','BR-011',
'Independent pair of monolithic parallel-leaf compliant finger modules.
 Shared native part/module instances; external gripper actuator outsid
e scope. Whole-mm geometry,1mm webs,56mm straight span,12mm depth,32mm
 nominal contact gap. Undeformed CAD reference; material condition, el
astic range, fatigue and gripping force unassigned.',(#13868));
#13870=PRODUCT('Finger module','Finger module',$,(#13868));
#13871=PRODUCT('Mounting shoe','Mounting shoe',$,(#13868));
#13872=PRODUCT('Flexure finger','Flexure finger',$,(#13868));
#13873=PRODUCT('Contact pad','Contact pad',$,(#13868));
#13874=PRODUCT('Flat washer M5','Flat washer M5',$,(#13868));
#13875=PRODUCT('Socket head cap screw M5x25',
'Socket head cap screw M5x25',$,(#13868));
#13876=PRODUCT('Dowel pin','Dowel pin',$,(#13868));
#13877=PRESENTATION_STYLE_ASSIGNMENT((#13884));
#13878=PRESENTATION_STYLE_ASSIGNMENT((#13885));
#13879=PRESENTATION_STYLE_ASSIGNMENT((#13886));
#13880=PRESENTATION_STYLE_ASSIGNMENT((#13887));
#13881=PRESENTATION_STYLE_ASSIGNMENT((#13888));
#13882=PRESENTATION_STYLE_ASSIGNMENT((#13889));
#13883=PRESENTATION_STYLE_ASSIGNMENT((#13890));
#13884=SURFACE_STYLE_USAGE(.BOTH.,#13891);
#13885=SURFACE_STYLE_USAGE(.BOTH.,#13892);
#13886=SURFACE_STYLE_USAGE(.BOTH.,#13893);
#13887=SURFACE_STYLE_USAGE(.BOTH.,#13894);
#13888=SURFACE_STYLE_USAGE(.BOTH.,#13895);
#13889=SURFACE_STYLE_USAGE(.BOTH.,#13896);
#13890=SURFACE_STYLE_USAGE(.BOTH.,#13897);
#13891=SURFACE_SIDE_STYLE('',(#13898));
#13892=SURFACE_SIDE_STYLE('',(#13899));
#13893=SURFACE_SIDE_STYLE('',(#13900));
#13894=SURFACE_SIDE_STYLE('',(#13901));
#13895=SURFACE_SIDE_STYLE('',(#13902));
#13896=SURFACE_SIDE_STYLE('',(#13903));
#13897=SURFACE_SIDE_STYLE('',(#13904));
#13898=SURFACE_STYLE_FILL_AREA(#13905);
#13899=SURFACE_STYLE_FILL_AREA(#13906);
#13900=SURFACE_STYLE_FILL_AREA(#13907);
#13901=SURFACE_STYLE_FILL_AREA(#13908);
#13902=SURFACE_STYLE_FILL_AREA(#13909);
#13903=SURFACE_STYLE_FILL_AREA(#13910);
#13904=SURFACE_STYLE_FILL_AREA(#13911);
#13905=FILL_AREA_STYLE('Steel - Satin',(#13912));
#13906=FILL_AREA_STYLE('Dark blue',(#13913));
#13907=FILL_AREA_STYLE('Sky blue',(#13914));
#13908=FILL_AREA_STYLE('Light blue',(#13915));
#13909=FILL_AREA_STYLE('Light gray',(#13916));
#13910=FILL_AREA_STYLE('Dark gray',(#13917));
#13911=FILL_AREA_STYLE('Gray',(#13918));
#13912=FILL_AREA_STYLE_COLOUR('Steel - Satin',#13919);
#13913=FILL_AREA_STYLE_COLOUR('Dark blue',#13920);
#13914=FILL_AREA_STYLE_COLOUR('Sky blue',#13921);
#13915=FILL_AREA_STYLE_COLOUR('Light blue',#13922);
#13916=FILL_AREA_STYLE_COLOUR('Light gray',#13923);
#13917=FILL_AREA_STYLE_COLOUR('Dark gray',#13924);
#13918=FILL_AREA_STYLE_COLOUR('Gray',#13925);
#13919=COLOUR_RGB('Steel - Satin',0.627450980392157,0.627450980392157,0.627450980392157);
#13920=COLOUR_RGB('Dark blue',0.0901960784313725,0.270588235294118,0.513725490196078);
#13921=COLOUR_RGB('Sky blue',0.317647058823529,0.686274509803922,0.890196078431372);
#13922=COLOUR_RGB('Light blue',0.662745098039216,0.831372549019608,0.949019607843137);
#13923=COLOUR_RGB('Light gray',0.725490196078431,0.752941176470588,0.792156862745098);
#13924=COLOUR_RGB('Dark gray',0.250980392156863,0.282352941176471,0.32156862745098);
#13925=COLOUR_RGB('Gray',0.407843137254902,0.447058823529412,0.498039215686275);
ENDSEC;
END-ISO-10303-21;
